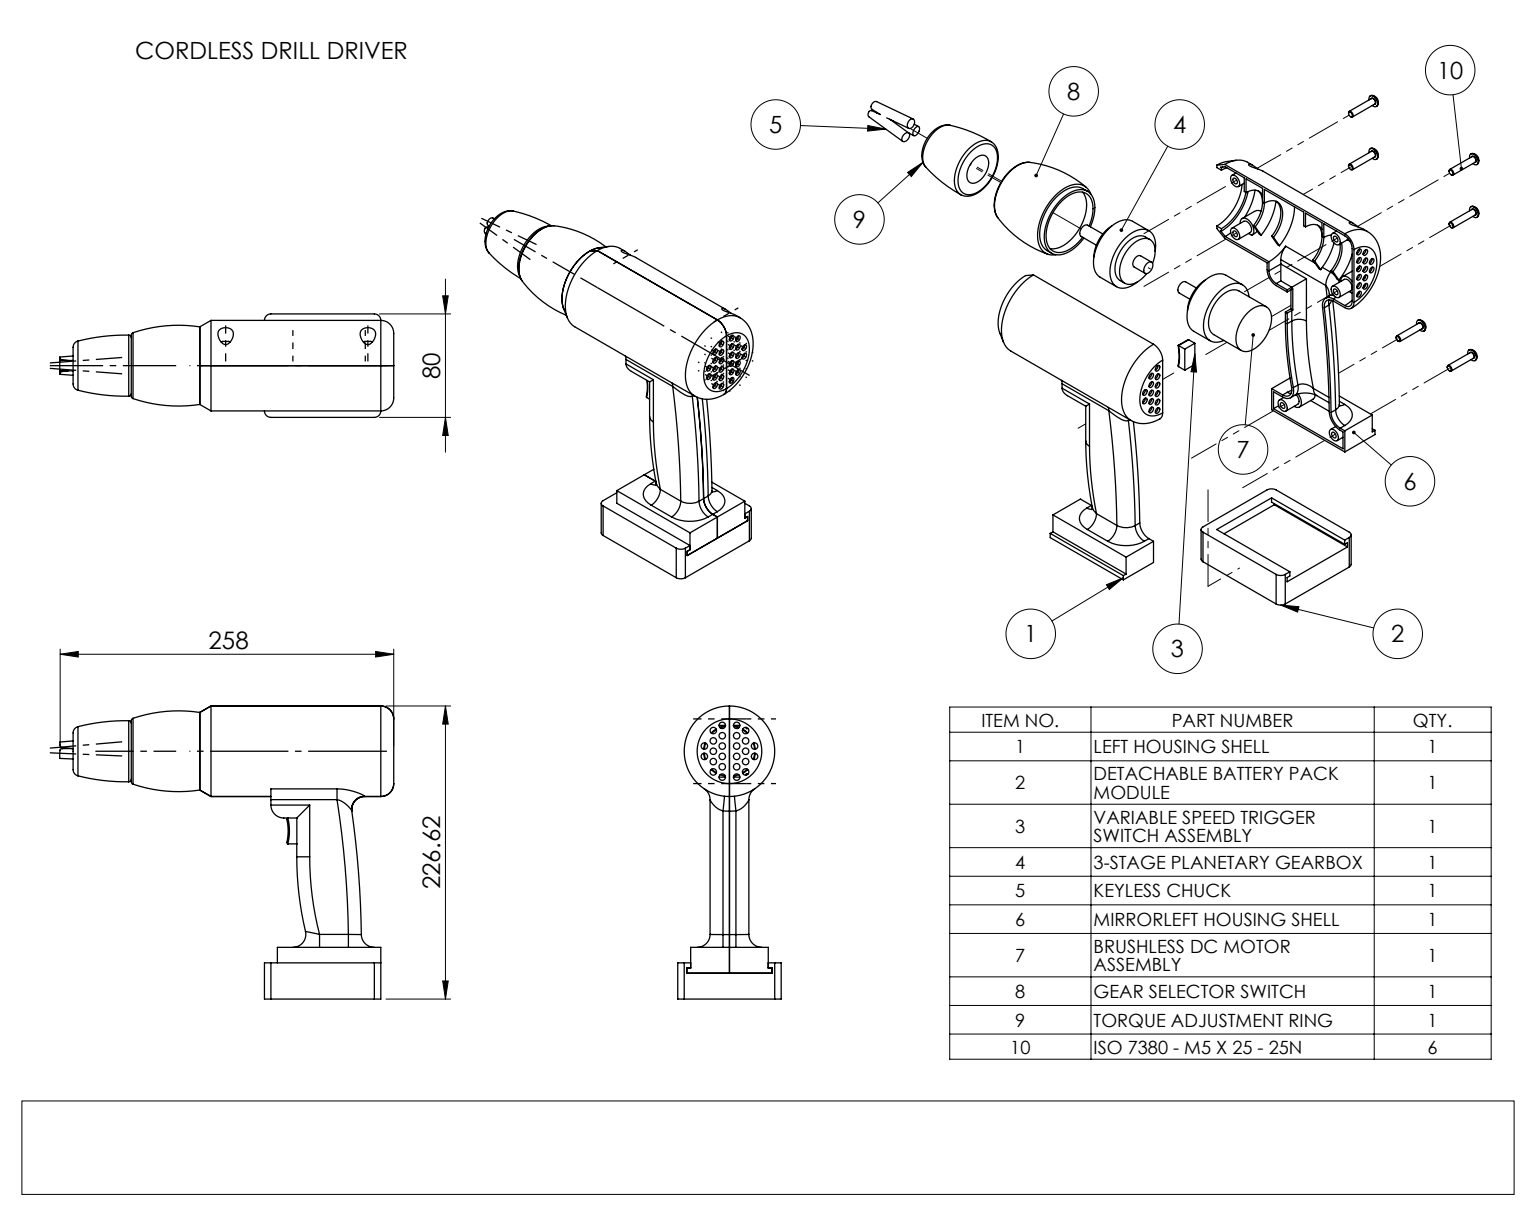
ISO-10303-21;
HEADER;
FILE_DESCRIPTION (('STEP AP214'),
    '1' );
FILE_NAME ('BR-801',
    '2026-10-05T20:22:16',
    ( '' ),
    ( '' ),
    'SwSTEP 2.0',
    'SolidWorks 2026',
    '' );
FILE_SCHEMA (( 'AUTOMOTIVE_DESIGN' ));
ENDSEC;

DATA;
#1 = B_SPLINE_CURVE_WITH_KNOTS ( 'NONE', 3,
 ( #12352, #9685, #8096, #1383, #14752, #16256, #12262, #13513, #2624, #1474, #13417, #8273, #9424, #10672, #226, #14828, #5538, #2709, #8188, #5630, #16442, #6792, #7929, #6603, #12185, #55, #13336, #5455, #10843, #10926, #4124, #11996, #2798, #16348, #13681, #6869, #9602, #15004, #9865, #16607, #8540, #3321, #16516, #15178, #7128, #4646, #4480, #11188, #15272, #15441 ),
 .UNSPECIFIED., .F., .F.,
 ( 4, 2, 2, 2, 2, 2, 2, 2, 2, 2, 2, 2, 2, 2, 2, 2, 2, 2, 2, 2, 2, 2, 2, 2, 4 ),
 ( 0.02172192739389853383, 0.02251948391625541862, 0.02331704043861230341, 0.02491215348332601748, 0.02650726652803973155, 0.02810237957275344908, 0.02969749261746715968, 0.03129260566218088069, 0.03209016218453770303, 0.03288771870689453231, 0.03328649696807296082, 0.03368527522925138240, 0.03448283175160819780, 0.03528038827396501320, 0.03567916653514340702, 0.03607794479632180085, 0.03687550131867862319, 0.03767305784103544553, 0.03847061436339226786, 0.03926817088574909020, 0.04086328393046270713, 0.04245839697517631711, 0.04405351001988992710, 0.04564862306460354402, 0.04724373610931716094 ),
 .UNSPECIFIED. ) ;
#2 = EDGE_CURVE ( 'NONE', #9188, #6176, #1844, .T. ) ;
#3 = AXIS2_PLACEMENT_3D ( 'NONE', #2045, #12839, #15664 ) ;
#4 = DIRECTION ( 'NONE',  ( 0.000000000000000000, 0.000000000000000000, -1.000000000000000000 ) ) ;
#5 = DIRECTION ( 'NONE',  ( 0.000000000000000000, 0.000000000000000000, 1.000000000000000000 ) ) ;
#6 = CARTESIAN_POINT ( 'NONE',  ( 27.15273249069231198, 18.00000000000000000, -20.88767039909325973 ) ) ;
#7 = CARTESIAN_POINT ( 'NONE',  ( 25.49876332522149625, 18.00000000000000000, -21.99427390110736624 ) ) ;
#8 = CYLINDRICAL_SURFACE ( 'NONE', #14336, 2.500000000000000444 ) ;
#9 = DIRECTION ( 'NONE',  ( -1.000000000000000000, 0.000000000000000000, 0.000000000000000000 ) ) ;
#10 = DIRECTION ( 'NONE',  ( -1.000000000000000000, -0.000000000000000000, -0.000000000000000000 ) ) ;
#11 = CARTESIAN_POINT ( 'NONE',  ( -70.00000000000000000, 171.6227766016838245, 0.000000000000000000 ) ) ;
#12 = ORIENTED_EDGE ( 'NONE', *, *, #6579, .T. ) ;
#13 = CARTESIAN_POINT ( 'NONE',  ( 16.03791926353974162, 127.7299327228906520, -9.742640703122631862 ) ) ;
#14 = CIRCLE ( 'NONE', #9896, 10.00000000000000178 ) ;
#15 = AXIS2_PLACEMENT_3D ( 'NONE', #2563, #7954, #5300 ) ;
#16 = ORIENTED_EDGE ( 'NONE', *, *, #13429, .F. ) ;
#17 = CARTESIAN_POINT ( 'NONE',  ( 196.0000000000000000, 191.6227766016837677, 3.071800142134975431 ) ) ;
#18 = CIRCLE ( 'NONE', #14435, 20.00000000000000355 ) ;
#19 = CYLINDRICAL_SURFACE ( 'NONE', #8941, 2.500000000000000444 ) ;
#20 = ORIENTED_EDGE ( 'NONE', *, *, #455, .F. ) ;
#21 = CARTESIAN_POINT ( 'NONE',  ( -12.77984573873758656, 20.00000000000230216, 11.87289823213939854 ) ) ;
#22 = CARTESIAN_POINT ( 'NONE',  ( 14.63750484765316706, 138.5418767416829837, 5.508738673615532377 ) ) ;
#23 = ORIENTED_EDGE ( 'NONE', *, *, #10609, .T. ) ;
#24 = CARTESIAN_POINT ( 'NONE',  ( 21.36708699129162881, 19.99999999999999645, 23.94811280430947420 ) ) ;
#25 = EDGE_CURVE ( 'NONE', #5251, #13584, #2714, .T. ) ;
#26 = AXIS2_PLACEMENT_3D ( 'NONE', #12707, #5981, #16782 ) ;
#27 = ORIENTED_EDGE ( 'NONE', *, *, #8063, .T. ) ;
#28 = AXIS2_PLACEMENT_3D ( 'NONE', #8615, #16596, #11271 ) ;
#29 = DIRECTION ( 'NONE',  ( 0.000000000000000000, 1.000000000000000000, 0.000000000000000000 ) ) ;
#30 = CARTESIAN_POINT ( 'NONE',  ( -15.00000000000002132, 100.0000000000000142, 4.999999999999999112 ) ) ;
#31 = DIRECTION ( 'NONE',  ( 0.000000000000000000, 0.000000000000000000, -1.000000000000000000 ) ) ;
#32 = CARTESIAN_POINT ( 'NONE',  ( -194.2319660531761656, 171.6227766016838245, -19.01029467089431080 ) ) ;
#33 = ADVANCED_FACE ( 'NONE', ( #8260 ), #11261, .F. ) ;
#34 = EDGE_CURVE ( 'NONE', #17370, #11003, #7190, .T. ) ;
#35 = ORIENTED_EDGE ( 'NONE', *, *, #2235, .F. ) ;
#36 = DIRECTION ( 'NONE',  ( -1.000000000000000000, 0.000000000000000000, 0.000000000000000000 ) ) ;
#37 = ORIENTED_EDGE ( 'NONE', *, *, #4762, .T. ) ;
#38 = CARTESIAN_POINT ( 'NONE',  ( -80.30638721710498373, 189.1234298779548624, -27.97726104294732963 ) ) ;
#39 = FACE_OUTER_BOUND ( 'NONE', #11505, .T. ) ;
#40 = AXIS2_PLACEMENT_3D ( 'NONE', #14825, #13678, #6691 ) ;
#41 = ORIENTED_EDGE ( 'NONE', *, *, #303, .F. ) ;
#42 = ORIENTED_EDGE ( 'NONE', *, *, #11841, .T. ) ;
#43 = ORIENTED_EDGE ( 'NONE', *, *, #9422, .T. ) ;
#44 = CARTESIAN_POINT ( 'NONE',  ( 9.986687348566183786, 132.8041431104223307, 14.33374896416919064 ) ) ;
#45 = ORIENTED_EDGE ( 'NONE', *, *, #7953, .F. ) ;
#46 = SHAPE_DEFINITION_REPRESENTATION ( #2904, #690 ) ;
#47 = CARTESIAN_POINT ( 'NONE',  ( -40.85786437626905609, 120.0000000000000142, 10.85786437626904721 ) ) ;
#48 = FACE_OUTER_BOUND ( 'NONE', #5615, .T. ) ;
#49 = PRODUCT_DEFINITION ( 'UNKNOWN', '', #15196, #232 ) ;
#50 = CARTESIAN_POINT ( 'NONE',  ( -48.00000000000000000, 143.0439382767972347, -16.49999999999984368 ) ) ;
#51 = AXIS2_PLACEMENT_3D ( 'NONE', #14892, #2772, #6847 ) ;
#52 = DIRECTION ( 'NONE',  ( 0.000000000000000000, 0.000000000000000000, -1.000000000000000000 ) ) ;
#53 = CARTESIAN_POINT ( 'NONE',  ( -80.79725519073433304, 151.5627461462769929, 26.20297826401936803 ) ) ;
#54 = ORIENTED_EDGE ( 'NONE', *, *, #3388, .T. ) ;
#55 = CARTESIAN_POINT ( 'NONE',  ( -79.71276265205243305, 202.6220268295897711, -16.24950730846250835 ) ) ;
#56 = CARTESIAN_POINT ( 'NONE',  ( 14.34366722128227067, 129.4994645064758174, 11.74322308516846647 ) ) ;
#57 = CARTESIAN_POINT ( 'NONE',  ( -95.00000000000000000, 171.6227766016838245, 0.000000000000000000 ) ) ;
#58 = CARTESIAN_POINT ( 'NONE',  ( -43.00000000000000000, 144.1839557653416080, 18.33333333333335702 ) ) ;
#59 = PLANE ( 'NONE',  #13735 ) ;
#60 = DIRECTION ( 'NONE',  ( 1.000000000000000000, 0.000000000000000000, 0.000000000000000000 ) ) ;
#61 = EDGE_CURVE ( 'NONE', #735, #11290, #4368, .T. ) ;
#62 = ORIENTED_EDGE ( 'NONE', *, *, #6340, .T. ) ;
#63 = FACE_OUTER_BOUND ( 'NONE', #17014, .T. ) ;
#64 = ORIENTED_EDGE ( 'NONE', *, *, #1601, .F. ) ;
#65 = SHAPE_REPRESENTATION_RELATIONSHIP ( 'NONE' , 'NONE' ,  #7924, #8036 ) ;
#66 = LINE ( 'NONE', #2892, #16980 ) ;
#67 = DIRECTION ( 'NONE',  ( 8.673617379884037937E-17, 0.000000000000000000, 1.000000000000000000 ) ) ;
#68 = DIRECTION ( 'NONE',  ( 0.000000000000000000, 0.000000000000000000, 1.000000000000000000 ) ) ;
#69 = CARTESIAN_POINT ( 'NONE',  ( 0.000000000000000000, 20.00000000000000000, 25.00000000000000000 ) ) ;
#70 = EDGE_LOOP ( 'NONE', ( #17465, #2421, #13202, #13512 ) ) ;
#71 = DIRECTION ( 'NONE',  ( -1.000000000000000000, 0.000000000000000000, 0.000000000000000000 ) ) ;
#72 = CARTESIAN_POINT ( 'NONE',  ( -48.00000000000000000, 191.6227766016837961, 1.224646799147353454E-15 ) ) ;
#73 = DIRECTION ( 'NONE',  ( 1.000000000000000000, 0.000000000000000000, 0.000000000000000000 ) ) ;
#74 =( NAMED_UNIT ( * ) PLANE_ANGLE_UNIT ( ) SI_UNIT ( $, .RADIAN. ) );
#75 = CARTESIAN_POINT ( 'NONE',  ( 15.93460003626540100, 136.8193095811535045, -3.708327557688629206 ) ) ;
#76 = ADVANCED_FACE ( 'NONE', ( #15069 ), #3033, .F. ) ;
#77 = EDGE_CURVE ( 'NONE', #13658, #4758, #14864, .T. ) ;
#78 = EDGE_CURVE ( 'NONE', #10896, #7127, #13853, .T. ) ;
#79 = ORIENTED_EDGE ( 'NONE', *, *, #12627, .T. ) ;
#80 = DIRECTION ( 'NONE',  ( 1.000000000000000000, 0.000000000000000000, 0.000000000000000000 ) ) ;
#81 = EDGE_CURVE ( 'NONE', #4275, #9730, #165, .T. ) ;
#82 = LINE ( 'NONE', #2908, #5241 ) ;
#83 = ORIENTED_EDGE ( 'NONE', *, *, #15385, .F. ) ;
#84 = CARTESIAN_POINT ( 'NONE',  ( -74.45226540305546337, 194.3303362407250177, -26.63481108765543581 ) ) ;
#85 = DIRECTION ( 'NONE',  ( -1.000000000000000000, -0.000000000000000000, -0.000000000000000000 ) ) ;
#86 = APPLICATION_CONTEXT ( 'automotive_design' ) ;
#87 = DIRECTION ( 'NONE',  ( 0.000000000000000000, 0.000000000000000000, 1.000000000000000000 ) ) ;
#88 = CARTESIAN_POINT ( 'NONE',  ( 24.94691999498327206, 18.00000000000000711, -22.32501294936691139 ) ) ;
#89 = CARTESIAN_POINT ( 'NONE',  ( 23.77503517897901375, 18.00000000000000000, -22.95135521423614833 ) ) ;
#90 = CARTESIAN_POINT ( 'NONE',  ( 37.50000000000000711, 196.6227766016838245, -35.00200000000000244 ) ) ;
#91 = LINE ( 'NONE', #4168, #1104 ) ;
#92 = CARTESIAN_POINT ( 'NONE',  ( 2.370000000000000551, 0.000000000000000000, 0.000000000000000000 ) ) ;
#93 = CARTESIAN_POINT ( 'NONE',  ( 26.85005685037350176, 141.4992599418080772, -17.82476597062854040 ) ) ;
#94 = ORIENTED_EDGE ( 'NONE', *, *, #1318, .F. ) ;
#95 = CARTESIAN_POINT ( 'NONE',  ( 6.927042533203191965, 134.0880917650273716, -15.00000000000000533 ) ) ;
#96 = EDGE_LOOP ( 'NONE', ( #1824, #2335, #11852, #6103 ) ) ;
#97 = DIRECTION ( 'NONE',  ( 0.000000000000000000, 0.000000000000000000, 1.000000000000000000 ) ) ;
#98 = CARTESIAN_POINT ( 'NONE',  ( 225.0000000000000000, 89.99999999999997158, -4.999999999999999112 ) ) ;
#99 = ORIENTED_EDGE ( 'NONE', *, *, #10624, .F. ) ;
#100 = PLANE ( 'NONE',  #16536 ) ;
#101 = LINE ( 'NONE', #8243, #15842 ) ;
#102 = VERTEX_POINT ( 'NONE', #8434 ) ;
#103 = DIRECTION ( 'NONE',  ( 0.000000000000000000, 0.000000000000000000, 1.000000000000000000 ) ) ;
#104 = ORIENTED_EDGE ( 'NONE', *, *, #3991, .F. ) ;
#105 = LINE ( 'NONE', #5601, #6122 ) ;
#106 = DIRECTION ( 'NONE',  ( -1.000000000000000000, 0.000000000000000000, 0.000000000000000000 ) ) ;
#107 = CARTESIAN_POINT ( 'NONE',  ( 33.99999999999998579, 9.999999999999998224, -35.00000000000000000 ) ) ;
#108 = ORIENTED_EDGE ( 'NONE', *, *, #12256, .F. ) ;
#109 = DIRECTION ( 'NONE',  ( -0.000000000000000000, -1.000000000000000000, -0.000000000000000000 ) ) ;
#110 = ORIENTED_EDGE ( 'NONE', *, *, #17517, .F. ) ;
#111 = LINE ( 'NONE', #8166, #1932 ) ;
#112 = EDGE_CURVE ( 'NONE', #17297, #3029, #16627, .T. ) ;
#113 = ORIENTED_EDGE ( 'NONE', *, *, #13886, .F. ) ;
#114 = EDGE_CURVE ( 'NONE', #730, #9326, #14586, .T. ) ;
#115 = CARTESIAN_POINT ( 'NONE',  ( -78.86500048027876630, 189.1866491494219815, -27.93804624201380804 ) ) ;
#116 = DIRECTION ( 'NONE',  ( 0.000000000000000000, 0.000000000000000000, 1.000000000000000000 ) ) ;
#117 =( BOUNDED_SURFACE ( )  B_SPLINE_SURFACE ( 3, 2, ( 
 ( #14255, #2119, #7358 ),
 ( #807, #6197, #12760 ),
 ( #632, #11415, #4699 ),
 ( #16827, #8771, #2299 ),
 ( #9106, #17259, #13450 ),
 ( #5135, #5041, #10344 ),
 ( #3799, #16120, #1322 ),
 ( #15926, #965, #13280 ),
 ( #13364, #6550, #2476 ),
 ( #14512, #14600, #10434 ),
 ( #15848, #1058, #6637 ),
 ( #11850, #2379, #3721 ),
 ( #6458, #16018, #11941 ),
 ( #8042, #15754, #7870 ),
 ( #7772, #5213, #10523 ),
 ( #10610, #6729, #9194 ),
 ( #13185, #1148, #17343 ),
 ( #3900, #9284, #12126 ),
 ( #3631, #4951, #3997 ),
 ( #14695, #11759, #2575 ),
 ( #7961, #1231, #9021 ),
 ( #14436, #7692, #9377 ),
 ( #13099, #12030, #17435 ),
 ( #6362, #5310, #17170 ),
 ( #14779, #10704, #2651 ),
 ( #13711, #13812, #9715 ),
 ( #11051, #256, #7075 ),
 ( #1415, #4329, #341 ),
 ( #4156, #8392, #9541 ),
 ( #8220, #1582, #3039 ) ),
 .UNSPECIFIED., .F., .F., .F. ) 
 B_SPLINE_SURFACE_WITH_KNOTS ( ( 4, 2, 2, 2, 2, 2, 2, 2, 2, 2, 2, 2, 2, 2, 4 ),
 ( 3, 3 ),
 ( 0.01165250788892075590, 0.01579789672993321681, 0.01787059115043944726, 0.01890693836069256423, 0.01994328557094567772, 0.02408867441195813863, 0.02616136883246436562, 0.02823406325297059608, 0.03030675767347682653, 0.03237945209398305352, 0.03652484093499551443, 0.03859753535550174142, 0.03963388256575485491, 0.04067022977600797534, 0.04481561861702043625 ),
 ( 0.000000000000000000, 1.000000000000000000 ),
 .UNSPECIFIED. ) 
 GEOMETRIC_REPRESENTATION_ITEM ( )  RATIONAL_B_SPLINE_SURFACE ( (
 ( 1.000000000000000000, 0.8819171036881968684, 1.000000000000000000),
 ( 1.000000000000000000, 0.8793942645247271317, 1.000000000000000000),
 ( 1.000000000000000000, 0.8749458316895473153, 1.000000000000000000),
 ( 1.000000000000000000, 0.8656814021268807169, 1.000000000000000000),
 ( 1.000000000000000000, 0.8621600075895787807, 1.000000000000000000),
 ( 1.000000000000000000, 0.8562492930711512740, 1.000000000000000000),
 ( 1.000000000000000000, 0.8541736901086096623, 1.000000000000000000),
 ( 1.000000000000000000, 0.8498659178638878764, 1.000000000000000000),
 ( 1.000000000000000000, 0.8476283308600994770, 1.000000000000000000),
 ( 1.000000000000000000, 0.8360458749413697266, 1.000000000000000000),
 ( 1.000000000000000000, 0.8255221978283152628, 1.000000000000000000),
 ( 1.000000000000000000, 0.8082270345000643896, 1.000000000000000000),
 ( 1.000000000000000000, 0.8022128341713220534, 1.000000000000000000),
 ( 1.000000000000000000, 0.7899684886175323273, 1.000000000000000000),
 ( 1.000000000000000000, 0.7837128169312477244, 1.000000000000000000),
 ( 1.000000000000000000, 0.7710263478628327505, 1.000000000000000000),
 ( 1.000000000000000000, 0.7645952338537677084, 1.000000000000000000),
 ( 1.000000000000000000, 0.7516613202047349729, 1.000000000000000000),
 ( 1.000000000000000000, 0.7451386183435962929, 1.000000000000000000),
 ( 1.000000000000000000, 0.7257808243687768890, 1.000000000000000000),
 ( 1.000000000000000000, 0.7133953845776382918, 1.000000000000000000),
 ( 1.000000000000000000, 0.6965170042221158209, 1.000000000000000000),
 ( 1.000000000000000000, 0.6911767420096451842, 1.000000000000000000),
 ( 1.000000000000000000, 0.6837405640632109316, 1.000000000000000000),
 ( 1.000000000000000000, 0.6813577907324296357, 1.000000000000000000),
 ( 1.000000000000000000, 0.6768117804540668692, 1.000000000000000000),
 ( 1.000000000000000000, 0.6746439590912666207, 1.000000000000000000),
 ( 1.000000000000000000, 0.6645663254999827352, 1.000000000000000000),
 ( 1.000000000000000000, 0.6588263891900785207, 1.000000000000000000),
 ( 1.000000000000000000, 0.6558243695371216431, 1.000000000000000000) ) ) 
 REPRESENTATION_ITEM ( '' )  SURFACE ( )  );
#118 = VERTEX_POINT ( 'NONE', #16766 ) ;
#119 = ORIENTED_EDGE ( 'NONE', *, *, #7483, .T. ) ;
#120 = ORIENTED_EDGE ( 'NONE', *, *, #14822, .T. ) ;
#121 = AXIS2_PLACEMENT_3D ( 'NONE', #12390, #5748, #16650 ) ;
#122 = AXIS2_PLACEMENT_3D ( 'NONE', #11876, #6482, #6572 ) ;
#123 = PLANE ( 'NONE',  #15795 ) ;
#124 = CARTESIAN_POINT ( 'NONE',  ( 10.15450428991780285, 132.7081580017661224, 14.27405243007192581 ) ) ;
#125 = ADVANCED_FACE ( 'NONE', ( #16843, #6296, #6218, #3209, #822 ), #15422, .T. ) ;
#126 = ORIENTED_EDGE ( 'NONE', *, *, #14248, .F. ) ;
#127 = CARTESIAN_POINT ( 'NONE',  ( 27.99999999999998224, 9.999999999999998224, -18.74999999999999645 ) ) ;
#128 = DIRECTION ( 'NONE',  ( -1.000000000000000000, -0.000000000000000000, -0.000000000000000000 ) ) ;
#129 = DIRECTION ( 'NONE',  ( 0.000000000000000000, 0.000000000000000000, 1.000000000000000000 ) ) ;
#130 = CARTESIAN_POINT ( 'NONE',  ( 22.12508471281541134, 29.85770821936580433, -8.546410110412809402 ) ) ;
#131 = CARTESIAN_POINT ( 'NONE',  ( 39.99999999999998579, 5.659323622547703371E-16, -33.00000000000000000 ) ) ;
#132 = CARTESIAN_POINT ( 'NONE',  ( -24.99999999999999289, 100.0000000000000142, 0.000000000000000000 ) ) ;
#133 = CIRCLE ( 'NONE', #1548, 2.499999999999998668 ) ;
#134 = VERTEX_POINT ( 'NONE', #6129 ) ;
#135 = CYLINDRICAL_SURFACE ( 'NONE', #5598, 8.000000000000007105 ) ;
#136 = CIRCLE ( 'NONE', #10306, 12.00000000000000000 ) ;
#137 = CARTESIAN_POINT ( 'NONE',  ( 34.80468147095351128, 20.00000000000000000, -7.619145204522578041 ) ) ;
#138 = ADVANCED_FACE ( 'NONE', ( #7376, #14017 ), #15677, .T. ) ;
#139 = LINE ( 'NONE', #14923, #9291 ) ;
#140 = FACE_OUTER_BOUND ( 'NONE', #14292, .T. ) ;
#141 = ORIENTED_EDGE ( 'NONE', *, *, #16389, .F. ) ;
#142 = CARTESIAN_POINT ( 'NONE',  ( -82.50000000000001421, 196.6227766016838245, 0.000000000000000000 ) ) ;
#143 = ORIENTED_EDGE ( 'NONE', *, *, #14951, .F. ) ;
#144 = EDGE_CURVE ( 'NONE', #16894, #7251, #3853, .T. ) ;
#145 = DIRECTION ( 'NONE',  ( 0.000000000000000000, -0.000000000000000000, -1.000000000000000000 ) ) ;
#146 = EDGE_CURVE ( 'NONE', #17383, #9593, #6108, .T. ) ;
#147 = ORIENTED_EDGE ( 'NONE', *, *, #10920, .T. ) ;
#148 =( LENGTH_UNIT ( ) NAMED_UNIT ( * ) SI_UNIT ( .MILLI., .METRE. ) );
#149 = CARTESIAN_POINT ( 'NONE',  ( 15.95607457768013404, 136.6882381644216196, -2.475222843548684715 ) ) ;
#150 = LINE ( 'NONE', #5809, #16568 ) ;
#151 = CARTESIAN_POINT ( 'NONE',  ( 1.559999999999998943, 1.732050807568885631, 0.000000000000000000 ) ) ;
#152 = VERTEX_POINT ( 'NONE', #7624 ) ;
#153 = CYLINDRICAL_SURFACE ( 'NONE', #9538, 24.99999999999999645 ) ;
#154 = CARTESIAN_POINT ( 'NONE',  ( 196.0000000000000000, 175.6227766016838530, 21.92820660268601074 ) ) ;
#155 = EDGE_CURVE ( 'NONE', #4227, #5635, #15763, .T. ) ;
#156 = CARTESIAN_POINT ( 'NONE',  ( -3.000000000000000888, 171.6227766016838245, 0.000000000000000000 ) ) ;
#157 = STYLED_ITEM ( 'NONE', ( #14231 ), #11475 ) ;
#158 = CIRCLE ( 'NONE', #16310, 33.00000000000000000 ) ;
#159 = CARTESIAN_POINT ( 'NONE',  ( 20.41303537792882139, 140.1262507166239573, -15.26811025958205015 ) ) ;
#160 = VERTEX_POINT ( 'NONE', #11356 ) ;
#161 = DIRECTION ( 'NONE',  ( 0.000000000000000000, 0.000000000000000000, -1.000000000000000000 ) ) ;
#162 = FACE_OUTER_BOUND ( 'NONE', #7033, .T. ) ;
#163 = EDGE_LOOP ( 'NONE', ( #2201, #7278 ) ) ;
#164 = CARTESIAN_POINT ( 'NONE',  ( -76.63222342921277175, 191.6397216241467163, -28.71272404723380234 ) ) ;
#165 = CIRCLE ( 'NONE', #16002, 2.500000000000002220 ) ;
#166 = AXIS2_PLACEMENT_3D ( 'NONE', #4042, #9504, #12180 ) ;
#167 = CARTESIAN_POINT ( 'NONE',  ( -7.379000772444994638, 30.00000000000000000, 25.00000000000000000 ) ) ;
#168 = CIRCLE ( 'NONE', #8369, 12.00000000000000000 ) ;
#169 = DIRECTION ( 'NONE',  ( -1.000000000000000000, -0.000000000000000000, 0.000000000000000000 ) ) ;
#170 = CARTESIAN_POINT ( 'NONE',  ( 17.00000000000000000, 154.3022685259950038, 9.999999999999900524 ) ) ;
#171 = CARTESIAN_POINT ( 'NONE',  ( -40.00000000000000000, 8.000000000000000000, -40.00000000000000000 ) ) ;
#172 = CARTESIAN_POINT ( 'NONE',  ( 15.46067906867578046, 29.98929614515185804, 13.00000000000000533 ) ) ;
#173 = ADVANCED_FACE ( 'NONE', ( #16682 ), #11434, .F. ) ;
#174 = EDGE_CURVE ( 'NONE', #6874, #11959, #3395, .T. ) ;
#175 = FACE_OUTER_BOUND ( 'NONE', #10777, .T. ) ;
#176 = EDGE_CURVE ( 'NONE', #5792, #4284, #10914, .T. ) ;
#177 = DIRECTION ( 'NONE',  ( 0.000000000000000000, -1.000000000000000000, 0.000000000000000000 ) ) ;
#178 = ORIENTED_EDGE ( 'NONE', *, *, #2632, .F. ) ;
#179 = CARTESIAN_POINT ( 'NONE',  ( 49.99999999999998579, 187.6227766016837961, 12.50000337241049309 ) ) ;
#180 = EDGE_LOOP ( 'NONE', ( #8241, #14719, #12649, #3237 ) ) ;
#181 = CARTESIAN_POINT ( 'NONE',  ( -50.00000000000000000, 171.6227766016838245, 0.000000000000000000 ) ) ;
#182 = CIRCLE ( 'NONE', #5556, 239.9999999999999716 ) ;
#183 = AXIS2_PLACEMENT_3D ( 'NONE', #7714, #6580, #13125 ) ;
#184 = CARTESIAN_POINT ( 'NONE',  ( -50.00000000000000000, 204.6227766016838245, 2.020667218593133100E-15 ) ) ;
#185 = VECTOR ( 'NONE', #14301, 1000.000000000000114 ) ;
#186 = ORIENTED_EDGE ( 'NONE', *, *, #12034, .F. ) ;
#187 = CARTESIAN_POINT ( 'NONE',  ( -25.16839285024614625, 19.99999999999999645, 15.12082343620048519 ) ) ;
#188 = AXIS2_PLACEMENT_3D ( 'NONE', #16749, #13998, #10087 ) ;
#189 = DIRECTION ( 'NONE',  ( 0.000000000000000000, 1.000000000000000000, 0.000000000000000000 ) ) ;
#190 = VERTEX_POINT ( 'NONE', #15337 ) ;
#191 = CARTESIAN_POINT ( 'NONE',  ( 36.34904889156061358, 150.6223998522366685, -25.45681811525070515 ) ) ;
#192 = ORIENTED_EDGE ( 'NONE', *, *, #2912, .T. ) ;
#193 = CARTESIAN_POINT ( 'NONE',  ( -95.00000000000000000, 171.6227766016838245, 0.000000000000000000 ) ) ;
#194 = CARTESIAN_POINT ( 'NONE',  ( -40.00000000000000000, 4.000000000000000000, -30.00000000000000711 ) ) ;
#195 = DIRECTION ( 'NONE',  ( 0.1091791256177803149, 0.9940220915700701543, 0.000000000000000000 ) ) ;
#196 = EDGE_LOOP ( 'NONE', ( #16642, #10984, #15395, #3760 ) ) ;
#197 = EDGE_CURVE ( 'NONE', #6224, #17297, #182, .T. ) ;
#198 = VECTOR ( 'NONE', #10876, 1000.000000000000000 ) ;
#199 = CYLINDRICAL_SURFACE ( 'NONE', #1827, 5.000000000000000888 ) ;
#200 = AXIS2_PLACEMENT_3D ( 'NONE', #10939, #4055, #145 ) ;
#201 = ORIENTED_EDGE ( 'NONE', *, *, #8299, .T. ) ;
#202 = FACE_OUTER_BOUND ( 'NONE', #3833, .T. ) ;
#203 = ORIENTED_EDGE ( 'NONE', *, *, #13054, .T. ) ;
#204 = CARTESIAN_POINT ( 'NONE',  ( -87.34717144291671787, 195.0632477915243896, -23.23525722188765741 ) ) ;
#205 = LINE ( 'NONE', #13586, #10347 ) ;
#206 = B_SPLINE_CURVE_WITH_KNOTS ( 'NONE', 3,
 ( #3287, #16669, #445, #365, #283, #11345, #15732, #8689, #8323, #15407, #4447, #11249, #548, #7099, #5687, #9833, #14096, #7178, #17064, #1960, #11419, #12580, #4538, #1702, #8592, #1874 ),
 .UNSPECIFIED., .F., .F.,
 ( 4, 2, 2, 2, 2, 2, 2, 2, 2, 2, 2, 2, 4 ),
 ( 0.000000000000000000, 0.002002783134349999609, 0.004005566268699999218, 0.008011132537399998435, 0.01001391567174999414, 0.01201669880609998985, 0.01602226507479997952, 0.01802504820914997002, 0.02002783134349995706, 0.02403339761219993806, 0.02603618074654992856, 0.02803896388089991906, 0.03204453014959990353 ),
 .UNSPECIFIED. ) ;
#207 = CARTESIAN_POINT ( 'NONE',  ( 48.00000000000000711, 175.6227766016838245, -5.571800142134975431 ) ) ;
#208 = ORIENTED_EDGE ( 'NONE', *, *, #12480, .F. ) ;
#209 = VERTEX_POINT ( 'NONE', #8951 ) ;
#210 = CARTESIAN_POINT ( 'NONE',  ( 15.00000000000000000, 204.6227766016838245, -2.020667218593133100E-15 ) ) ;
#211 = AXIS2_PLACEMENT_3D ( 'NONE', #6627, #17422, #13266 ) ;
#212 = CARTESIAN_POINT ( 'NONE',  ( 17.58250999372313927, 125.2198453307267414, 1.671679122699602171 ) ) ;
#213 = DIRECTION ( 'NONE',  ( -1.000000000000000000, 0.000000000000000000, 0.000000000000000000 ) ) ;
#214 = DIRECTION ( 'NONE',  ( 0.000000000000000000, -1.000000000000000000, -6.123233995736762338E-17 ) ) ;
#215 = CIRCLE ( 'NONE', #1923, 5.000000000000018652 ) ;
#216 = VERTEX_POINT ( 'NONE', #8789 ) ;
#217 = SHAPE_DEFINITION_REPRESENTATION ( #9683, #10772 ) ;
#218 = DIRECTION ( 'NONE',  ( 1.000000000000000000, 0.000000000000000000, -0.000000000000000000 ) ) ;
#219 = ADVANCED_FACE ( 'NONE', ( #14195 ), #2057, .T. ) ;
#220 = CARTESIAN_POINT ( 'NONE',  ( 32.50000000000000711, 146.6227766016838245, -16.00000000000000000 ) ) ;
#221 = CARTESIAN_POINT ( 'NONE',  ( 17.51497691750854813, 29.94811823131043127, -12.57651788136221072 ) ) ;
#222 = CARTESIAN_POINT ( 'NONE',  ( -40.00000000000000000, 0.000000000000000000, -33.00000000000000711 ) ) ;
#223 = CARTESIAN_POINT ( 'NONE',  ( 27.44407568426044364, 136.8394969516870958, 3.888888888888887063 ) ) ;
#224 = PRODUCT_DEFINITION_SHAPE ( 'NONE', 'NONE',  #17527 ) ;
#225 = ORIENTED_EDGE ( 'NONE', *, *, #16801, .F. ) ;
#226 = CARTESIAN_POINT ( 'NONE',  ( -83.14616744761717371, 201.7487681645689577, -17.82060658420953203 ) ) ;
#227 = DIRECTION ( 'NONE',  ( 0.000000000000000000, 0.000000000000000000, 1.000000000000000000 ) ) ;
#228 = CARTESIAN_POINT ( 'NONE',  ( -72.50000000000002842, 146.6227766016838245, -35.00200000000000244 ) ) ;
#229 = CARTESIAN_POINT ( 'NONE',  ( -208.1430079281944074, 172.4097984991905150, 5.932774073184737595 ) ) ;
#230 = VECTOR ( 'NONE', #15433, 1000.000000000000000 ) ;
#231 = CARTESIAN_POINT ( 'NONE',  ( -45.00000000000000000, 122.0000000000000142, 15.00000000000000000 ) ) ;
#232 = PRODUCT_DEFINITION_CONTEXT ( 'detailed design', #10711, 'design' ) ;
#233 = VERTEX_POINT ( 'NONE', #10201 ) ;
#234 = CARTESIAN_POINT ( 'NONE',  ( 48.00000000000000000, 171.6227766016838245, 0.000000000000000000 ) ) ;
#235 = EDGE_LOOP ( 'NONE', ( #13574, #321, #10866, #12718 ) ) ;
#236 = LINE ( 'NONE', #5641, #6716 ) ;
#237 = EDGE_LOOP ( 'NONE', ( #1431, #15859, #12881, #16657, #10889, #7991, #12906, #8862 ) ) ;
#238 = AXIS2_PLACEMENT_3D ( 'NONE', #16301, #6473, #17358 ) ;
#239 = CARTESIAN_POINT ( 'NONE',  ( 196.0000000000000000, 179.6227766016838245, 15.00000337241049486 ) ) ;
#240 = EDGE_CURVE ( 'NONE', #15883, #846, #6193, .T. ) ;
#241 = AXIS2_PLACEMENT_3D ( 'NONE', #3615, #7420, #699 ) ;
#242 = CARTESIAN_POINT ( 'NONE',  ( -95.00000000000000000, 171.6227766016838245, 0.000000000000000000 ) ) ;
#243 = VERTEX_POINT ( 'NONE', #13302 ) ;
#244 = CARTESIAN_POINT ( 'NONE',  ( -100.0000000000000000, 143.9321776784423150, -5.086680500673126297E-15 ) ) ;
#245 = ADVANCED_FACE ( 'NONE', ( #10458, #10362 ), #15773, .T. ) ;
#246 = DIRECTION ( 'NONE',  ( -0.000000000000000000, -0.000000000000000000, -1.000000000000000000 ) ) ;
#247 = FACE_BOUND ( 'NONE', #9621, .T. ) ;
#248 = ADVANCED_FACE ( 'NONE', ( #14797, #17095 ), #7707, .F. ) ;
#249 = FILL_AREA_STYLE_COLOUR ( '', #15123 ) ;
#250 = EDGE_CURVE ( 'NONE', #2500, #6282, #1348, .T. ) ;
#251 = AXIS2_PLACEMENT_3D ( 'NONE', #3268, #2197, #881 ) ;
#252 = CIRCLE ( 'NONE', #11000, 2.500000000000000000 ) ;
#253 = CARTESIAN_POINT ( 'NONE',  ( 14.17453072134883030, 137.9246278893784847, -11.09209212451273352 ) ) ;
#254 = VERTEX_POINT ( 'NONE', #2317 ) ;
#255 = FACE_BOUND ( 'NONE', #9759, .T. ) ;
#256 = CARTESIAN_POINT ( 'NONE',  ( 14.12141184870282196, 138.6801925718470443, -3.743222489502411321 ) ) ;
#257 = ORIENTED_EDGE ( 'NONE', *, *, #3098, .T. ) ;
#258 = DIRECTION ( 'NONE',  ( 0.000000000000000000, 0.000000000000000000, 1.000000000000000000 ) ) ;
#259 = CARTESIAN_POINT ( 'NONE',  ( -80.44925623706835438, 190.6352453962669813, -29.38582951075080985 ) ) ;
#260 = DIRECTION ( 'NONE',  ( -0.000000000000000000, -0.000000000000000000, -1.000000000000000000 ) ) ;
#261 = CIRCLE ( 'NONE', #1953, 5.000000000000007994 ) ;
#262 = CIRCLE ( 'NONE', #2818, 2.499999999999998668 ) ;
#263 = CARTESIAN_POINT ( 'NONE',  ( -43.00000000000000000, 130.0000000000000000, -15.00000000000000000 ) ) ;
#264 = AXIS2_PLACEMENT_3D ( 'NONE', #14224, #8819, #502 ) ;
#265 = DIRECTION ( 'NONE',  ( -0.000000000000000000, -0.000000000000000000, -1.000000000000000000 ) ) ;
#266 = CARTESIAN_POINT ( 'NONE',  ( 19.82112781281243130, 29.90253658286262350, 11.35562597552217845 ) ) ;
#267 = CARTESIAN_POINT ( 'NONE',  ( 11.38015211399644500, 143.8700659084811093, -17.85516819212570638 ) ) ;
#268 = CARTESIAN_POINT ( 'NONE',  ( 34.99999999999999289, -20.00000000000000000, 39.99999999999998579 ) ) ;
#269 = ORIENTED_EDGE ( 'NONE', *, *, #1597, .F. ) ;
#270 = ORIENTED_EDGE ( 'NONE', *, *, #12627, .F. ) ;
#271 = CARTESIAN_POINT ( 'NONE',  ( 24.41196201396447663, 19.99999999999999645, -8.570466955472159754 ) ) ;
#272 = CIRCLE ( 'NONE', #13562, 28.26633746182136164 ) ;
#273 = VECTOR ( 'NONE', #8822, 1000.000000000000000 ) ;
#274 = CARTESIAN_POINT ( 'NONE',  ( 24.00000000000000000, 196.6227766016838245, -16.00000000000000000 ) ) ;
#275 = ORIENTED_EDGE ( 'NONE', *, *, #16105, .F. ) ;
#276 = CARTESIAN_POINT ( 'NONE',  ( -15.53366225407947354, 31.76144936975385136, 11.66511309525283835 ) ) ;
#277 = CIRCLE ( 'NONE', #6204, 20.00000000000000355 ) ;
#278 = DIRECTION ( 'NONE',  ( 1.000000000000000000, 0.000000000000000000, 0.000000000000000000 ) ) ;
#279 = EDGE_CURVE ( 'NONE', #3972, #817, #6479, .T. ) ;
#280 = ORIENTED_EDGE ( 'NONE', *, *, #8979, .F. ) ;
#281 = EDGE_CURVE ( 'NONE', #6275, #15920, #15863, .T. ) ;
#282 = CARTESIAN_POINT ( 'NONE',  ( -50.00000000000000000, 171.6227766016838245, 0.000000000000000000 ) ) ;
#283 = CARTESIAN_POINT ( 'NONE',  ( -27.70723240392776887, 18.00000000000000000, 8.328409877367404235 ) ) ;
#284 = CARTESIAN_POINT ( 'NONE',  ( -68.00000000000000000, 171.6227766016838245, 24.99999999999999289 ) ) ;
#285 = DIRECTION ( 'NONE',  ( 0.000000000000000000, 0.000000000000000000, -1.000000000000000000 ) ) ;
#286 = AXIS2_PLACEMENT_3D ( 'NONE', #5190, #14314, #1029 ) ;
#287 = CIRCLE ( 'NONE', #5084, 23.57392898041429774 ) ;
#288 = LINE ( 'NONE', #8596, #3725 ) ;
#289 = PLANE ( 'NONE',  #9740 ) ;
#290 = CIRCLE ( 'NONE', #10181, 33.00000000000000000 ) ;
#291 = DIRECTION ( 'NONE',  ( -1.000000000000000000, 0.000000000000000000, 0.000000000000000000 ) ) ;
#292 = EDGE_LOOP ( 'NONE', ( #6190, #15449, #12115, #5130, #6244, #17037, #12475 ) ) ;
#293 = CARTESIAN_POINT ( 'NONE',  ( 225.0000000000000000, 89.99999999999997158, -4.999999999999999112 ) ) ;
#294 = EDGE_LOOP ( 'NONE', ( #280, #3412, #14427, #14815 ) ) ;
#295 = CARTESIAN_POINT ( 'NONE',  ( -72.55951795904178425, 195.6584727333609521, -22.61345334826514630 ) ) ;
#296 = FACE_BOUND ( 'NONE', #6496, .T. ) ;
#297 = DIRECTION ( 'NONE',  ( 0.000000000000000000, 0.000000000000000000, 1.000000000000000000 ) ) ;
#298 = ORIENTED_EDGE ( 'NONE', *, *, #12256, .T. ) ;
#299 = EDGE_LOOP ( 'NONE', ( #9917, #12342, #13408, #14524 ) ) ;
#300 = CARTESIAN_POINT ( 'NONE',  ( -90.80384757729339640, 204.6227766016838245, 0.000000000000000000 ) ) ;
#301 = CIRCLE ( 'NONE', #9619, 24.99999999999999645 ) ;
#302 = EDGE_CURVE ( 'NONE', #14819, #8809, #14878, .T. ) ;
#303 = EDGE_CURVE ( 'NONE', #12797, #10037, #6701, .T. ) ;
#304 = FACE_OUTER_BOUND ( 'NONE', #8211, .T. ) ;
#305 = EDGE_CURVE ( 'NONE', #13136, #4801, #3737, .T. ) ;
#306 = CARTESIAN_POINT ( 'NONE',  ( 16.12877328687227774, 136.8349817083154676, 4.209125965272636272 ) ) ;
#307 = ORIENTED_EDGE ( 'NONE', *, *, #3862, .T. ) ;
#308 = PLANE ( 'NONE',  #8782 ) ;
#309 = DIRECTION ( 'NONE',  ( -0.000000000000000000, -0.000000000000000000, -1.000000000000000000 ) ) ;
#310 = CARTESIAN_POINT ( 'NONE',  ( -50.00000000000000000, 171.6227766016838245, 0.000000000000000000 ) ) ;
#311 = CARTESIAN_POINT ( 'NONE',  ( -32.66708739526796279, 119.0000000000141824, -4.722170599054655860 ) ) ;
#312 = FACE_OUTER_BOUND ( 'NONE', #3125, .T. ) ;
#313 = VERTEX_POINT ( 'NONE', #2399 ) ;
#314 = CARTESIAN_POINT ( 'NONE',  ( -31.89848094669885725, 100.0271397714182342, 5.500000000000000000 ) ) ;
#315 = CIRCLE ( 'NONE', #13889, 10.00000000000000178 ) ;
#316 = FACE_OUTER_BOUND ( 'NONE', #16097, .T. ) ;
#317 = DIRECTION ( 'NONE',  ( -1.000000000000000000, 0.000000000000000000, 0.000000000000000000 ) ) ;
#318 = CARTESIAN_POINT ( 'NONE',  ( -45.00000000000000000, 130.0000000000000000, 0.000000000000000000 ) ) ;
#319 = ORIENTED_EDGE ( 'NONE', *, *, #15425, .T. ) ;
#320 = EDGE_CURVE ( 'NONE', #5614, #12465, #7243, .T. ) ;
#321 = ORIENTED_EDGE ( 'NONE', *, *, #1465, .F. ) ;
#322 = PLANE ( 'NONE',  #5083 ) ;
#323 = ORIENTED_EDGE ( 'NONE', *, *, #15869, .T. ) ;
#324 = DIRECTION ( 'NONE',  ( 0.8571673013836870192, 1.049727191973306873E-16, -0.5150380737757234151 ) ) ;
#325 = AXIS2_PLACEMENT_3D ( 'NONE', #12063, #5342, #16056 ) ;
#326 = ORIENTED_EDGE ( 'NONE', *, *, #14886, .T. ) ;
#327 = PRESENTATION_STYLE_ASSIGNMENT (( #16528 ) ) ;
#328 = CARTESIAN_POINT ( 'NONE',  ( -16.30611068361787019, 32.76923076923078781, -4.999999999999999112 ) ) ;
#329 = LINE ( 'NONE', #4059, #732 ) ;
#330 = DIRECTION ( 'NONE',  ( 0.000000000000000000, 0.000000000000000000, 1.000000000000000000 ) ) ;
#331 = CARTESIAN_POINT ( 'NONE',  ( -31.66708739526795924, 120.0000000000000284, -5.500000000000000000 ) ) ;
#332 = EDGE_LOOP ( 'NONE', ( #9563, #15113 ) ) ;
#333 = CARTESIAN_POINT ( 'NONE',  ( -100.0000000000000000, 171.6227766016838245, 0.000000000000000000 ) ) ;
#334 = LINE ( 'NONE', #11212, #17228 ) ;
#335 = FACE_BOUND ( 'NONE', #8357, .T. ) ;
#336 = ADVANCED_FACE ( 'NONE', ( #9394 ), #7794, .F. ) ;
#337 = EDGE_CURVE ( 'NONE', #3754, #14218, #4437, .T. ) ;
#338 = CARTESIAN_POINT ( 'NONE',  ( 25.02538947967125793, 138.3580044269788800, -10.92703196337285299 ) ) ;
#339 = ORIENTED_EDGE ( 'NONE', *, *, #6159, .F. ) ;
#340 = CARTESIAN_POINT ( 'NONE',  ( -74.59180618087658843, 149.2475623141791061, -26.91697313366100985 ) ) ;
#341 = CARTESIAN_POINT ( 'NONE',  ( 27.25143353317894324, 139.0964629073462220, -5.659441210211040740 ) ) ;
#342 = ORIENTED_EDGE ( 'NONE', *, *, #14528, .T. ) ;
#343 = FILL_AREA_STYLE_COLOUR ( '', #7574 ) ;
#344 = CARTESIAN_POINT ( 'NONE',  ( -77.78509460342800708, 191.0296277843087296, -29.12775510238319399 ) ) ;
#345 = EDGE_CURVE ( 'NONE', #10903, #313, #5234, .T. ) ;
#346 = DIRECTION ( 'NONE',  ( 0.000000000000000000, 0.000000000000000000, -1.000000000000000000 ) ) ;
#347 = CARTESIAN_POINT ( 'NONE',  ( 25.75727093772393061, 193.9598103731634637, 24.29383909379279061 ) ) ;
#348 = CARTESIAN_POINT ( 'NONE',  ( -116.4755503550297107, 171.6227766016838245, 0.000000000000000000 ) ) ;
#349 = CARTESIAN_POINT ( 'NONE',  ( 0.000000000000000000, 3.061616997868382155E-16, -2.499999999999999112 ) ) ;
#350 = CARTESIAN_POINT ( 'NONE',  ( -50.00000000000000000, 171.6227766016838245, 24.99999999999999289 ) ) ;
#351 = CARTESIAN_POINT ( 'NONE',  ( -79.90458729923355463, 201.6232707959690060, 13.74664867617476460 ) ) ;
#352 = DIRECTION ( 'NONE',  ( 1.000000000000000000, 0.000000000000000000, 0.000000000000000000 ) ) ;
#353 = ORIENTED_EDGE ( 'NONE', *, *, #661, .F. ) ;
#354 = ORIENTED_EDGE ( 'NONE', *, *, #25, .T. ) ;
#355 = CARTESIAN_POINT ( 'NONE',  ( 34.93420767782698988, 19.99999999999999645, -6.321724734770472587 ) ) ;
#356 = B_SPLINE_CURVE_WITH_KNOTS ( 'NONE', 3,
 ( #7684, #11748, #15744, #10079, #15575, #885, #3452, #9097, #3622, #16818, #9013, #14426, #12830, #2290, #14173, #621, #2110, #11499, #13092, #10426, #17157, #3713, #6274, #15486, #7510, #10172, #957, #3367, #2372, #8840, #14245, #8761, #2034, #12919, #15652, #11589, #16996, #4863, #6352, #3529, #14505, #8920, #11664, #8122, #3791, #2468, #11934, #9443, #9277, #16010 ),
 .UNSPECIFIED., .F., .F.,
 ( 4, 2, 2, 2, 2, 2, 2, 2, 2, 2, 2, 2, 2, 2, 2, 2, 2, 2, 2, 2, 2, 2, 2, 2, 4 ),
 ( 0.02172192739389855118, 0.02251948391625536658, 0.02331704043861218198, 0.02491215348332581278, 0.02650726652803944358, 0.02810237957275307438, 0.02969749261746670171, 0.03129260566218033252, 0.03209016218453714098, 0.03288771870689394250, 0.03328649696807235020, 0.03368527522925075790, 0.03448283175160756636, 0.03528038827396437482, 0.03567916653514278946, 0.03607794479632120410, 0.03687550131867804726, 0.03767305784103488348, 0.03847061436339171969, 0.03926817088574855591, 0.04086328393046227692, 0.04245839697517599792, 0.04405351001988971893, 0.04564862306460343994, 0.04724373610931716094 ),
 .UNSPECIFIED. ) ;
#357 = DIRECTION ( 'NONE',  ( 8.673617379884037937E-17, 0.000000000000000000, 1.000000000000000000 ) ) ;
#358 = EDGE_LOOP ( 'NONE', ( #12471, #2318, #7218, #8842 ) ) ;
#359 = CARTESIAN_POINT ( 'NONE',  ( -27.98221281347032274, 19.99999999999999645, 4.999999999999996447 ) ) ;
#360 = PRODUCT_RELATED_PRODUCT_CATEGORY ( 'part', '', ( #8716 ) ) ;
#361 = CYLINDRICAL_SURFACE ( 'NONE', #2522, 248.0000000000000000 ) ;
#362 = ORIENTED_EDGE ( 'NONE', *, *, #2234, .T. ) ;
#363 = CARTESIAN_POINT ( 'NONE',  ( 37.21337428997476593, 198.7412861714591941, -18.82352572523459600 ) ) ;
#364 = EDGE_CURVE ( 'NONE', #14743, #3326, #2669, .T. ) ;
#365 = CARTESIAN_POINT ( 'NONE',  ( -27.81025873171734375, 18.00000000000000355, 7.666431193274476641 ) ) ;
#366 = DIRECTION ( 'NONE',  ( -1.000000000000000000, -0.000000000000000000, -0.000000000000000000 ) ) ;
#367 = CARTESIAN_POINT ( 'NONE',  ( -206.3689767832464668, 174.5534660175772785, 3.987129972734268168 ) ) ;
#368 = DIRECTION ( 'NONE',  ( -1.000000000000000000, -0.000000000000000000, -0.000000000000000000 ) ) ;
#369 = CARTESIAN_POINT ( 'NONE',  ( -100.0000000000000000, 142.8100939375178200, -16.63501009223129756 ) ) ;
#370 = FACE_OUTER_BOUND ( 'NONE', #15719, .T. ) ;
#371 = ORIENTED_EDGE ( 'NONE', *, *, #3539, .F. ) ;
#372 = CARTESIAN_POINT ( 'NONE',  ( 24.48161681970857018, 138.6020828307752879, -11.64873334838780572 ) ) ;
#373 = EDGE_CURVE ( 'NONE', #8849, #8796, #6836, .T. ) ;
#374 = VERTEX_POINT ( 'NONE', #16306 ) ;
#375 = CARTESIAN_POINT ( 'NONE',  ( -68.00000000000000000, 171.6227766016838245, -19.49999999999999645 ) ) ;
#376 = CARTESIAN_POINT ( 'NONE',  ( -8.461393309425545795, 30.35704578695612099, -12.95687587100684368 ) ) ;
#377 = EDGE_LOOP ( 'NONE', ( #3921, #10271, #6852, #11471 ) ) ;
#378 = ORIENTED_EDGE ( 'NONE', *, *, #1221, .T. ) ;
#379 = LINE ( 'NONE', #5779, #16244 ) ;
#380 = CARTESIAN_POINT ( 'NONE',  ( 15.95607457770042181, 136.6882381644217048, 2.475222843549475638 ) ) ;
#381 = CARTESIAN_POINT ( 'NONE',  ( 13.38958197704232056, 130.3612470323695902, 12.52688079436099144 ) ) ;
#382 = ORIENTED_EDGE ( 'NONE', *, *, #10198, .F. ) ;
#383 = DIRECTION ( 'NONE',  ( 3.469446951953614189E-16, -1.000000000000000000, 0.000000000000000000 ) ) ;
#384 = LINE ( 'NONE', #14028, #11479 ) ;
#385 = CARTESIAN_POINT ( 'NONE',  ( -81.89019958151206424, 191.9899036175949618, 25.96511099662697930 ) ) ;
#386 = DIRECTION ( 'NONE',  ( 0.000000000000000000, 0.000000000000000000, 1.000000000000000000 ) ) ;
#387 = CARTESIAN_POINT ( 'NONE',  ( 17.50698843878764777, 29.94827730614627725, 12.57924512168886011 ) ) ;
#388 = DIRECTION ( 'NONE',  ( 0.000000000000000000, -0.4999999999999997224, 0.8660254037844387076 ) ) ;
#389 = EDGE_LOOP ( 'NONE', ( #662, #9822, #5339, #17357 ) ) ;
#390 = DIRECTION ( 'NONE',  ( 0.000000000000000000, 0.000000000000000000, 1.000000000000000000 ) ) ;
#391 = ADVANCED_FACE ( 'NONE', ( #9825 ), #19, .F. ) ;
#392 = ADVANCED_FACE ( 'NONE', ( #6907 ), #7804, .F. ) ;
#393 = DIRECTION ( 'NONE',  ( 1.000000000000000000, 0.000000000000000000, 0.000000000000000000 ) ) ;
#394 = EDGE_CURVE ( 'NONE', #12251, #2211, #12340, .T. ) ;
#395 = CARTESIAN_POINT ( 'NONE',  ( 27.15273249069231198, 19.99999999999999645, -20.88767039909325973 ) ) ;
#396 = CARTESIAN_POINT ( 'NONE',  ( -206.1506185320109239, 176.5415102007174255, 53.79077198841061147 ) ) ;
#397 = DIRECTION ( 'NONE',  ( -0.000000000000000000, -0.000000000000000000, 1.000000000000000000 ) ) ;
#398 = AXIS2_PLACEMENT_3D ( 'NONE', #9363, #2641, #5198 ) ;
#399 = VERTEX_POINT ( 'NONE', #184 ) ;
#400 = ORIENTED_EDGE ( 'NONE', *, *, #61, .T. ) ;
#401 = CARTESIAN_POINT ( 'NONE',  ( 8.997728150919979129, 132.8900016178789372, 12.55705910147062099 ) ) ;
#402 = EDGE_LOOP ( 'NONE', ( #8088, #12658, #10491, #2591 ) ) ;
#403 = EDGE_LOOP ( 'NONE', ( #5681, #2940, #16094, #11500 ) ) ;
#404 = CARTESIAN_POINT ( 'NONE',  ( 30.00000000000000355, 196.6227766016838245, 35.00200000000000244 ) ) ;
#405 = FACE_OUTER_BOUND ( 'NONE', #3645, .T. ) ;
#406 = CIRCLE ( 'NONE', #6632, 12.00000000000000000 ) ;
#407 = CARTESIAN_POINT ( 'NONE',  ( -96.00000000000001421, 201.6227766016838245, 0.000000000000000000 ) ) ;
#408 = CARTESIAN_POINT ( 'NONE',  ( -24.99999999999999289, 100.0000000000000142, -15.00000000000000000 ) ) ;
#409 = AXIS2_PLACEMENT_3D ( 'NONE', #3562, #17022, #2059 ) ;
#410 = CARTESIAN_POINT ( 'NONE',  ( 29.53214135918722505, 18.00000000000000000, -18.68621337607990185 ) ) ;
#411 = ORIENTED_EDGE ( 'NONE', *, *, #16163, .T. ) ;
#412 = CARTESIAN_POINT ( 'NONE',  ( 27.31119513844540947, 142.3932571782017931, 15.32207027268389510 ) ) ;
#413 = DIRECTION ( 'NONE',  ( 0.000000000000000000, 0.000000000000000000, 1.000000000000000000 ) ) ;
#414 = FACE_BOUND ( 'NONE', #1666, .T. ) ;
#415 = LINE ( 'NONE', #5821, #443 ) ;
#416 = AXIS2_PLACEMENT_3D ( 'NONE', #17010, #17352, #6371 ) ;
#417 = PLANE ( 'NONE',  #8765 ) ;
#418 = AXIS2_PLACEMENT_3D ( 'NONE', #14483, #7741, #8010 ) ;
#419 = ORIENTED_EDGE ( 'NONE', *, *, #3121, .F. ) ;
#420 = CARTESIAN_POINT ( 'NONE',  ( -50.00000000000000000, 191.6227766016837961, -1.224646799147353454E-15 ) ) ;
#421 = EDGE_LOOP ( 'NONE', ( #5552, #2069, #2676, #10202 ) ) ;
#422 = CARTESIAN_POINT ( 'NONE',  ( -75.17085894487867392, 193.0398713882428012, -27.68487141596273915 ) ) ;
#423 = CARTESIAN_POINT ( 'NONE',  ( 40.00000000000000711, 146.6227766016838245, 0.000000000000000000 ) ) ;
#424 = LINE ( 'NONE', #5834, #8946 ) ;
#425 = ADVANCED_FACE ( 'NONE', ( #5501 ), #4977, .T. ) ;
#426 = FACE_BOUND ( 'NONE', #13934, .T. ) ;
#427 = VECTOR ( 'NONE', #13768, 1000.000000000000000 ) ;
#428 = CARTESIAN_POINT ( 'NONE',  ( -95.00000000000000000, 171.6227766016838245, 0.000000000000000000 ) ) ;
#429 = DIRECTION ( 'NONE',  ( -0.000000000000000000, -0.000000000000000000, -1.000000000000000000 ) ) ;
#430 = MECHANICAL_DESIGN_GEOMETRIC_PRESENTATION_REPRESENTATION (  '', ( #7494 ), #12593 ) ;
#431 = CARTESIAN_POINT ( 'NONE',  ( -80.14161447679168759, 201.6221756766236979, 13.74903839801200789 ) ) ;
#432 = AXIS2_PLACEMENT_3D ( 'NONE', #5586, #6655, #5500 ) ;
#433 = FACE_BOUND ( 'NONE', #13642, .T. ) ;
#434 = ORIENTED_EDGE ( 'NONE', *, *, #16551, .T. ) ;
#435 = EDGE_LOOP ( 'NONE', ( #4715, #8702, #12659, #943, #16358, #4658 ) ) ;
#436 = CARTESIAN_POINT ( 'NONE',  ( 24.40970717605596718, 29.87515913883691354, -8.215055496182330330 ) ) ;
#437 = CARTESIAN_POINT ( 'NONE',  ( 27.04079503965286690, 139.2301514590222098, -6.313402927548398047 ) ) ;
#438 = ORIENTED_EDGE ( 'NONE', *, *, #11422, .T. ) ;
#439 = CARTESIAN_POINT ( 'NONE',  ( -14.83003349241583813, 19.99999999999883116, 8.298189366023557056 ) ) ;
#440 = DIRECTION ( 'NONE',  ( -1.000000000000000000, 0.000000000000000000, 0.000000000000000000 ) ) ;
#441 = VECTOR ( 'NONE', #9945, 1000.000000000000000 ) ;
#442 = ORIENTED_EDGE ( 'NONE', *, *, #11491, .T. ) ;
#443 = VECTOR ( 'NONE', #15203, 1000.000000000000000 ) ;
#444 = DIRECTION ( 'NONE',  ( -1.000000000000000000, -0.000000000000000000, -0.000000000000000000 ) ) ;
#445 = CARTESIAN_POINT ( 'NONE',  ( -27.94760966554430937, 18.00000000000000355, 6.338314452217974626 ) ) ;
#446 = EDGE_CURVE ( 'NONE', #9960, #12327, #12060, .T. ) ;
#447 = DIRECTION ( 'NONE',  ( -0.000000000000000000, -0.000000000000000000, -1.000000000000000000 ) ) ;
#448 = CARTESIAN_POINT ( 'NONE',  ( -207.5170152892447959, 175.0764231502095072, 3.989746324742934558 ) ) ;
#449 = PLANE ( 'NONE',  #5426 ) ;
#450 = CARTESIAN_POINT ( 'NONE',  ( -32.02886766642249228, 119.9418479153533781, 5.500000000000000888 ) ) ;
#451 = CARTESIAN_POINT ( 'NONE',  ( -74.40218896425085404, 141.6107120069882512, -13.74530841833676220 ) ) ;
#452 = AXIS2_PLACEMENT_3D ( 'NONE', #1785, #447, #9743 ) ;
#453 = VERTEX_POINT ( 'NONE', #5588 ) ;
#454 = DIRECTION ( 'NONE',  ( 1.000000000000000000, -0.000000000000000000, -0.000000000000000000 ) ) ;
#455 = EDGE_CURVE ( 'NONE', #7796, #10705, #11208, .T. ) ;
#456 = AXIS2_PLACEMENT_3D ( 'NONE', #11979, #6311, #7995 ) ;
#457 = VERTEX_POINT ( 'NONE', #10979 ) ;
#458 = EDGE_CURVE ( 'NONE', #11543, #11435, #15731, .T. ) ;
#459 = CARTESIAN_POINT ( 'NONE',  ( -95.00000000000000000, 171.6227766016838245, 0.000000000000000000 ) ) ;
#460 = EDGE_CURVE ( 'NONE', #8505, #14597, #2443, .T. ) ;
#461 = DIRECTION ( 'NONE',  ( -0.000000000000000000, -0.000000000000000000, -1.000000000000000000 ) ) ;
#462 = ORIENTED_EDGE ( 'NONE', *, *, #5545, .F. ) ;
#463 = DIRECTION ( 'NONE',  ( 1.000000000000000000, 0.000000000000000000, 0.000000000000000000 ) ) ;
#464 = CYLINDRICAL_SURFACE ( 'NONE', #1410, 2.499999999999998668 ) ;
#465 = CARTESIAN_POINT ( 'NONE',  ( 24.34257225596279639, 138.6622241066778543, 11.80661878326775494 ) ) ;
#466 = VECTOR ( 'NONE', #9041, 1000.000000000000000 ) ;
#467 = AXIS2_PLACEMENT_3D ( 'NONE', #16027, #3907, #7967 ) ;
#468 = ORIENTED_EDGE ( 'NONE', *, *, #15742, .T. ) ;
#469 = ITEM_DEFINED_TRANSFORMATION ( 'NONE', 'NONE', #8959,  #3583 ) ;
#470 = ADVANCED_FACE ( 'NONE', ( #12227 ), #3105, .T. ) ;
#471 = LINE ( 'NONE', #14027, #16068 ) ;
#472 = VECTOR ( 'NONE', #10118, 1000.000000000000114 ) ;
#473 = PRESENTATION_LAYER_ASSIGNMENT (  '', '', ( #2461 ) ) ;
#474 = DIRECTION ( 'NONE',  ( -1.000000000000000000, 0.000000000000000000, 0.000000000000000000 ) ) ;
#475 = AXIS2_PLACEMENT_3D ( 'NONE', #11596, #1866, #6196 ) ;
#476 = CARTESIAN_POINT ( 'NONE',  ( -78.09342651567857274, 191.9854139975492160, 25.96938468333279104 ) ) ;
#477 = DIRECTION ( 'NONE',  ( -1.000000000000000000, -0.000000000000000000, -0.000000000000000000 ) ) ;
#478 = CARTESIAN_POINT ( 'NONE',  ( 19.81659905433974700, 29.90262535319825332, 11.35915249282563444 ) ) ;
#479 = CARTESIAN_POINT ( 'NONE',  ( -7.379000772444995526, 30.00000000000000000, -13.00000000000000178 ) ) ;
#480 = ORIENTED_EDGE ( 'NONE', *, *, #11200, .F. ) ;
#481 = DIRECTION ( 'NONE',  ( 0.000000000000000000, 1.000000000000000000, 0.000000000000000000 ) ) ;
#482 = CARTESIAN_POINT ( 'NONE',  ( 2.370000000000000551, -4.750000000000000888, -5.817072295949928412E-16 ) ) ;
#483 = CARTESIAN_POINT ( 'NONE',  ( 32.91012024024373517, 19.99999999999999289, -13.86436652238006673 ) ) ;
#484 = DIRECTION ( 'NONE',  ( -1.000000000000000000, 0.000000000000000000, 0.000000000000000000 ) ) ;
#485 = CARTESIAN_POINT ( 'NONE',  ( -50.00000000000000000, 171.6227766016838245, 0.000000000000000000 ) ) ;
#486 = ORIENTED_EDGE ( 'NONE', *, *, #6340, .F. ) ;
#487 = AXIS2_PLACEMENT_3D ( 'NONE', #11537, #16029, #3909 ) ;
#488 = ORIENTED_EDGE ( 'NONE', *, *, #9995, .F. ) ;
#489 = VERTEX_POINT ( 'NONE', #13915 ) ;
#490 = ORIENTED_EDGE ( 'NONE', *, *, #17231, .F. ) ;
#491 = CIRCLE ( 'NONE', #16041, 33.00000000000000000 ) ;
#492 = CYLINDRICAL_SURFACE ( 'NONE', #1416, 10.00000000000000178 ) ;
#493 = ORIENTED_EDGE ( 'NONE', *, *, #9337, .F. ) ;
#494 = CARTESIAN_POINT ( 'NONE',  ( 40.00000000000000711, 171.6227766016838245, 0.000000000000000000 ) ) ;
#495 = EDGE_LOOP ( 'NONE', ( #13630, #14725, #1232, #7431, #16585, #10286, #6595, #15301, #1355, #7450, #11318, #10338 ) ) ;
#496 = EDGE_CURVE ( 'NONE', #16329, #13265, #6750, .T. ) ;
#497 = EDGE_CURVE ( 'NONE', #6006, #5256, #4292, .T. ) ;
#498 = DIRECTION ( 'NONE',  ( -1.000000000000000000, -0.000000000000000000, 0.000000000000000000 ) ) ;
#499 = EDGE_CURVE ( 'NONE', #9593, #12318, #8101, .T. ) ;
#500 = CIRCLE ( 'NONE', #10943, 10.00000000000000178 ) ;
#501 = CARTESIAN_POINT ( 'NONE',  ( 40.00000000000000711, 204.6227766016838245, -2.020667218593133100E-15 ) ) ;
#502 = DIRECTION ( 'NONE',  ( -1.000000000000000000, 0.000000000000000000, 0.000000000000000000 ) ) ;
#503 = CARTESIAN_POINT ( 'NONE',  ( -45.00000000000000000, 130.0000000000000000, -15.00000000000000000 ) ) ;
#504 = AXIS2_PLACEMENT_3D ( 'NONE', #14770, #8028, #16194 ) ;
#505 = AXIS2_PLACEMENT_3D ( 'NONE', #14744, #2617, #15707 ) ;
#506 = VECTOR ( 'NONE', #763, 1000.000000000000000 ) ;
#507 = ORIENTED_EDGE ( 'NONE', *, *, #5137, .F. ) ;
#508 = DIRECTION ( 'NONE',  ( -1.000000000000000000, -0.000000000000000000, -0.000000000000000000 ) ) ;
#509 = CARTESIAN_POINT ( 'NONE',  ( -192.9999999999999716, 171.6227766016838245, 0.000000000000000000 ) ) ;
#510 = DIRECTION ( 'NONE',  ( -1.000000000000000000, 0.000000000000000000, 0.000000000000000000 ) ) ;
#511 = CARTESIAN_POINT ( 'NONE',  ( -8.766611209710754693, 19.99999999999771916, -14.60748648876205458 ) ) ;
#512 = LINE ( 'NONE', #4502, #12581 ) ;
#513 = PRODUCT_DEFINITION_SHAPE ( 'NONE', 'NONE',  #17523 ) ;
#514 = CYLINDRICAL_SURFACE ( 'NONE', #16412, 6.000000000000005329 ) ;
#515 = CIRCLE ( 'NONE', #6739, 8.000000000000000000 ) ;
#516 = ORIENTED_EDGE ( 'NONE', *, *, #7943, .F. ) ;
#517 = CARTESIAN_POINT ( 'NONE',  ( -75.00000000000002842, 146.6227766016838245, 0.000000000000000000 ) ) ;
#518 = CIRCLE ( 'NONE', #8724, 4.000000000000001776 ) ;
#519 = ORIENTED_EDGE ( 'NONE', *, *, #4625, .F. ) ;
#520 = EDGE_CURVE ( 'NONE', #7447, #15746, #3010, .T. ) ;
#521 = FILL_AREA_STYLE_COLOUR ( '', #2206 ) ;
#522 = ADVANCED_FACE ( 'NONE', ( #13830 ), #1695, .F. ) ;
#523 = DIRECTION ( 'NONE',  ( 1.000000000000000000, 0.000000000000000000, 0.000000000000000000 ) ) ;
#524 = EDGE_LOOP ( 'NONE', ( #9216, #14969 ) ) ;
#525 = CARTESIAN_POINT ( 'NONE',  ( -725.0000000000000000, 30.00000000000000000, -25.00000000000000000 ) ) ;
#526 = CARTESIAN_POINT ( 'NONE',  ( 39.99999999999998579, 4.000000000000000000, -33.00000000000000000 ) ) ;
#527 = DIRECTION ( 'NONE',  ( 1.000000000000000000, -0.000000000000000000, -0.000000000000000000 ) ) ;
#528 = ORIENTED_EDGE ( 'NONE', *, *, #5545, .T. ) ;
#529 = CARTESIAN_POINT ( 'NONE',  ( 27.99999999999998224, 9.999999999999998224, 0.000000000000000000 ) ) ;
#530 = CARTESIAN_POINT ( 'NONE',  ( -77.50000000000001421, 196.6227766016838245, 10.00000000000000178 ) ) ;
#531 = AXIS2_PLACEMENT_3D ( 'NONE', #7704, #6212, #3646 ) ;
#532 = CARTESIAN_POINT ( 'NONE',  ( -79.43217333917553447, 201.5917424073650182, 13.81529814621275953 ) ) ;
#533 = CIRCLE ( 'NONE', #811, 21.61734737250326077 ) ;
#534 = SURFACE_STYLE_USAGE ( .BOTH. , #5674 ) ;
#535 = EDGE_LOOP ( 'NONE', ( #5840, #7471, #16377, #3579 ) ) ;
#536 = ORIENTED_EDGE ( 'NONE', *, *, #1514, .F. ) ;
#537 = CARTESIAN_POINT ( 'NONE',  ( 24.72170379509201865, 19.99999999999999645, -7.619165077982883894 ) ) ;
#538 = CARTESIAN_POINT ( 'NONE',  ( 19.59022622986824302, 142.1737554346910599, -14.89790021284453303 ) ) ;
#539 = VERTEX_POINT ( 'NONE', #274 ) ;
#540 = ADVANCED_FACE ( 'NONE', ( #12491 ), #2116, .T. ) ;
#541 = CARTESIAN_POINT ( 'NONE',  ( 35.00000000000000711, 146.6227766016838245, 35.00200000000000244 ) ) ;
#542 = CARTESIAN_POINT ( 'NONE',  ( -187.6513770290094385, 171.1853623553244006, 0.7576236986490064718 ) ) ;
#543 = AXIS2_PLACEMENT_3D ( 'NONE', #9206, #16030, #16296 ) ;
#544 = VERTEX_POINT ( 'NONE', #5945 ) ;
#545 = AXIS2_PLACEMENT_3D ( 'NONE', #15355, #5797, #5891 ) ;
#546 = PLANE ( 'NONE',  #7342 ) ;
#547 = AXIS2_PLACEMENT_3D ( 'NONE', #310, #15173, #4211 ) ;
#548 = CARTESIAN_POINT ( 'NONE',  ( -22.79696676584440596, 18.00000000000000711, 18.34105320469107170 ) ) ;
#549 = CYLINDRICAL_SURFACE ( 'NONE', #11760, 35.00000000000000000 ) ;
#550 = DIRECTION ( 'NONE',  ( 0.000000000000000000, 0.000000000000000000, 1.000000000000000000 ) ) ;
#551 = CARTESIAN_POINT ( 'NONE',  ( -7.379000772444995526, 18.00000000000000355, 12.99999999999999822 ) ) ;
#552 = DIRECTION ( 'NONE',  ( 1.000000000000000000, 0.000000000000000000, 0.000000000000000000 ) ) ;
#553 = CARTESIAN_POINT ( 'NONE',  ( -72.50000000000002842, 146.6227766016838245, -21.54065922853802562 ) ) ;
#554 = VERTEX_POINT ( 'NONE', #15318 ) ;
#555 = CYLINDRICAL_SURFACE ( 'NONE', #8157, 33.00000000000000000 ) ;
#556 = AXIS2_PLACEMENT_3D ( 'NONE', #15496, #7518, #2210 ) ;
#557 = VECTOR ( 'NONE', #9968, 1000.000000000000114 ) ;
#558 = AXIS2_PLACEMENT_3D ( 'NONE', #9560, #17361, #13561 ) ;
#559 = ORIENTED_EDGE ( 'NONE', *, *, #15927, .T. ) ;
#560 = CARTESIAN_POINT ( 'NONE',  ( -90.80384757729339640, 204.6227766016838245, 0.000000000000000000 ) ) ;
#561 = VECTOR ( 'NONE', #2674, 1000.000000000000000 ) ;
#562 = CARTESIAN_POINT ( 'NONE',  ( -26.10410744458347665, 18.00000000000000000, -13.37721135299797304 ) ) ;
#563 = ORIENTED_EDGE ( 'NONE', *, *, #11755, .F. ) ;
#564 = EDGE_CURVE ( 'NONE', #4853, #5097, #11488, .T. ) ;
#565 = CARTESIAN_POINT ( 'NONE',  ( 23.79315516583586643, 19.99999999999999645, 22.94240041036162836 ) ) ;
#566 = DIRECTION ( 'NONE',  ( 0.000000000000000000, 0.000000000000000000, -1.000000000000000000 ) ) ;
#567 = CARTESIAN_POINT ( 'NONE',  ( 15.80099858973940030, 127.9994182179736413, 10.08996921773076316 ) ) ;
#568 = AXIS2_PLACEMENT_3D ( 'NONE', #14760, #4313, #60 ) ;
#569 = AXIS2_PLACEMENT_3D ( 'NONE', #5580, #6650, #6830 ) ;
#570 = VERTEX_POINT ( 'NONE', #6023 ) ;
#571 = CARTESIAN_POINT ( 'NONE',  ( 37.99999999999999289, 2.000000000000000000, -8.789265611615818404E-15 ) ) ;
#572 = EDGE_CURVE ( 'NONE', #3368, #13835, #6120, .T. ) ;
#573 = CIRCLE ( 'NONE', #11580, 2.500000000000000444 ) ;
#574 = DIRECTION ( 'NONE',  ( 0.000000000000000000, 1.000000000000000000, 0.000000000000000000 ) ) ;
#575 = EDGE_CURVE ( 'NONE', #8346, #5702, #12911, .T. ) ;
#576 = DIRECTION ( 'NONE',  ( 0.000000000000000000, 0.000000000000000000, 1.000000000000000000 ) ) ;
#577 = DIRECTION ( 'NONE',  ( -1.000000000000000000, 1.040834085586084059E-15, 0.000000000000000000 ) ) ;
#578 = CARTESIAN_POINT ( 'NONE',  ( 17.01529014380724192, 17.99999999999942801, 12.76845467807931733 ) ) ;
#579 = CARTESIAN_POINT ( 'NONE',  ( -68.00000000000000000, 204.6227766016838245, 0.000000000000000000 ) ) ;
#580 = ORIENTED_EDGE ( 'NONE', *, *, #7866, .T. ) ;
#581 = CARTESIAN_POINT ( 'NONE',  ( -725.0000000000000000, 30.00000000000000000, 13.00000000000000000 ) ) ;
#582 = CARTESIAN_POINT ( 'NONE',  ( 225.0000000000000000, 89.99999999999997158, 4.999999999999999112 ) ) ;
#583 = VERTEX_POINT ( 'NONE', #4786 ) ;
#584 = DIRECTION ( 'NONE',  ( 0.000000000000000000, 0.000000000000000000, 1.000000000000000000 ) ) ;
#585 = CARTESIAN_POINT ( 'NONE',  ( -45.00000000000000000, 122.0000000000000142, -4.999999999999999112 ) ) ;
#586 = AXIS2_PLACEMENT_3D ( 'NONE', #156, #1313, #13701 ) ;
#587 = ORIENTED_EDGE ( 'NONE', *, *, #6448, .T. ) ;
#588 = VERTEX_POINT ( 'NONE', #3277 ) ;
#589 = ORIENTED_EDGE ( 'NONE', *, *, #4843, .T. ) ;
#590 = VECTOR ( 'NONE', #14056, 1000.000000000000000 ) ;
#591 = CARTESIAN_POINT ( 'NONE',  ( 11.63249183333955017, 139.6944596454877114, 10.84829254633709184 ) ) ;
#592 = ORIENTED_EDGE ( 'NONE', *, *, #11333, .F. ) ;
#593 = DIRECTION ( 'NONE',  ( 1.000000000000000000, 0.000000000000000000, 0.000000000000000000 ) ) ;
#594 = ORIENTED_EDGE ( 'NONE', *, *, #13777, .F. ) ;
#595 = SURFACE_STYLE_FILL_AREA ( #3338 ) ;
#596 = DIRECTION ( 'NONE',  ( 1.000000000000000000, 0.000000000000000000, 0.000000000000000000 ) ) ;
#597 = CARTESIAN_POINT ( 'NONE',  ( 13.91851620013868995, 127.9827558526829563, 9.294367823883964874 ) ) ;
#598 = DIRECTION ( 'NONE',  ( 0.000000000000000000, 1.000000000000000000, 0.000000000000000000 ) ) ;
#599 = AXIS2_PLACEMENT_3D ( 'NONE', #14005, #3199, #15140 ) ;
#600 = CARTESIAN_POINT ( 'NONE',  ( 25.00000000000000711, 146.6227766016838245, -12.99999999999999822 ) ) ;
#601 = B_SPLINE_CURVE_WITH_KNOTS ( 'NONE', 3,
 ( #15955, #13311, #9052, #1176 ),
 .UNSPECIFIED., .F., .F.,
 ( 4, 4 ),
 ( -6.324563032106999871E-06, 0.0003067249959486805411 ),
 .UNSPECIFIED. ) ;
#602 = ORIENTED_EDGE ( 'NONE', *, *, #14098, .F. ) ;
#603 = FACE_OUTER_BOUND ( 'NONE', #10174, .T. ) ;
#604 = LINE ( 'NONE', #8649, #6198 ) ;
#605 = PLANE ( 'NONE',  #3116 ) ;
#606 = CARTESIAN_POINT ( 'NONE',  ( -8.792264229871568304, 30.31966024794114745, -14.93731107458715357 ) ) ;
#607 = EDGE_CURVE ( 'NONE', #15092, #6530, #17001, .T. ) ;
#608 = AXIS2_PLACEMENT_3D ( 'NONE', #6490, #13127, #6395 ) ;
#609 = FACE_OUTER_BOUND ( 'NONE', #3195, .T. ) ;
#610 = ORIENTED_EDGE ( 'NONE', *, *, #4593, .T. ) ;
#611 = LINE ( 'NONE', #16893, #6704 ) ;
#612 = EDGE_CURVE ( 'NONE', #8809, #13930, #10178, .T. ) ;
#613 = EDGE_LOOP ( 'NONE', ( #6152, #6292 ) ) ;
#614 = CARTESIAN_POINT ( 'NONE',  ( -85.77828040291200296, 194.9977432358044496, -26.05112671349591125 ) ) ;
#615 = DIRECTION ( 'NONE',  ( 0.000000000000000000, 1.000000000000000000, 0.000000000000000000 ) ) ;
#616 = DIRECTION ( 'NONE',  ( 0.000000000000000000, 0.000000000000000000, 1.000000000000000000 ) ) ;
#617 = ORIENTED_EDGE ( 'NONE', *, *, #4810, .T. ) ;
#618 = DIRECTION ( 'NONE',  ( 0.000000000000000000, 0.000000000000000000, -1.000000000000000000 ) ) ;
#619 = CYLINDRICAL_SURFACE ( 'NONE', #11277, 6.000000000000005329 ) ;
#620 = CARTESIAN_POINT ( 'NONE',  ( -80.49255897422042949, 201.5998317580112200, 13.79770299781518972 ) ) ;
#621 = CARTESIAN_POINT ( 'NONE',  ( 27.40877793924366301, 202.0384121146825578, -17.31838511551978144 ) ) ;
#622 = ORIENTED_EDGE ( 'NONE', *, *, #10511, .F. ) ;
#623 = EDGE_CURVE ( 'NONE', #8295, #4586, #6392, .T. ) ;
#624 = EDGE_CURVE ( 'NONE', #1718, #6006, #5357, .T. ) ;
#625 = EDGE_CURVE ( 'NONE', #4234, #16058, #12632, .T. ) ;
#626 = ORIENTED_EDGE ( 'NONE', *, *, #13035, .T. ) ;
#627 = CARTESIAN_POINT ( 'NONE',  ( 30.00000000000001066, 146.6227766016838245, -35.00200000000000244 ) ) ;
#628 = EDGE_CURVE ( 'NONE', #9656, #12025, #15580, .T. ) ;
#629 = LINE ( 'NONE', #6194, #9795 ) ;
#630 = ORIENTED_EDGE ( 'NONE', *, *, #2454, .F. ) ;
#631 = DIRECTION ( 'NONE',  ( 0.000000000000000000, 0.000000000000000000, -1.000000000000000000 ) ) ;
#632 = CARTESIAN_POINT ( 'NONE',  ( 7.290380404777190293, 133.8591131982526008, -12.94327073059132971 ) ) ;
#633 = ORIENTED_EDGE ( 'NONE', *, *, #12413, .F. ) ;
#634 = CARTESIAN_POINT ( 'NONE',  ( -27.98221281347037959, 20.00000000000000000, 4.999999999999999112 ) ) ;
#635 = UNCERTAINTY_MEASURE_WITH_UNIT (LENGTH_MEASURE( 1.000000000000000082E-05 ), #4493, 'distance_accuracy_value', 'NONE');
#636 = CARTESIAN_POINT ( 'NONE',  ( -68.00000000000000000, 171.6227766016838245, 0.000000000000000000 ) ) ;
#637 = CARTESIAN_POINT ( 'NONE',  ( -207.6770884633517085, 166.3723159270569738, -1.150078995496658596 ) ) ;
#638 = CARTESIAN_POINT ( 'NONE',  ( -207.7508999721942189, 175.3364228813296108, 3.959069933371625716 ) ) ;
#639 = CARTESIAN_POINT ( 'NONE',  ( -12.55890155933014363, 17.99999999999884182, 7.515612101507582743 ) ) ;
#640 = LINE ( 'NONE', #12678, #3519 ) ;
#641 = CARTESIAN_POINT ( 'NONE',  ( -153.0000000000000284, 171.6227766016838245, 0.000000000000000000 ) ) ;
#642 = ORIENTED_EDGE ( 'NONE', *, *, #1514, .T. ) ;
#643 = FACE_OUTER_BOUND ( 'NONE', #1205, .T. ) ;
#644 = ORIENTED_EDGE ( 'NONE', *, *, #1969, .F. ) ;
#645 = CARTESIAN_POINT ( 'NONE',  ( 27.75000000000000000, 0.000000000000000000, 0.000000000000000000 ) ) ;
#646 = DIRECTION ( 'NONE',  ( 0.000000000000000000, 0.000000000000000000, 1.000000000000000000 ) ) ;
#647 = VERTEX_POINT ( 'NONE', #3540 ) ;
#648 = DIRECTION ( 'NONE',  ( 8.673617379884037937E-17, -2.891205793294676354E-16, -1.000000000000000000 ) ) ;
#649 = CARTESIAN_POINT ( 'NONE',  ( 24.93507336697333798, 29.86842105264641845, 5.660862367392566874 ) ) ;
#650 = CARTESIAN_POINT ( 'NONE',  ( 14.18611645313626290, 129.6406627243902676, 11.87032202561248617 ) ) ;
#651 = ORIENTED_EDGE ( 'NONE', *, *, #1422, .F. ) ;
#652 = ITEM_DEFINED_TRANSFORMATION ( 'NONE', 'NONE', #14353,  #3583 ) ;
#653 = DIRECTION ( 'NONE',  ( -1.000000000000000000, -0.000000000000000000, -0.000000000000000000 ) ) ;
#654 = DIRECTION ( 'NONE',  ( -1.000000000000000000, 0.000000000000000000, 0.000000000000000000 ) ) ;
#655 = CARTESIAN_POINT ( 'NONE',  ( -75.10425368493336862, 195.5720014495396981, 22.70655749026625614 ) ) ;
#656 = CYLINDRICAL_SURFACE ( 'NONE', #15299, 1.000000000000000888 ) ;
#657 =( REPRESENTATION_RELATIONSHIP ('NONE','NONE', #9723, #6585 ) REPRESENTATION_RELATIONSHIP_WITH_TRANSFORMATION ( #7289 )SHAPE_REPRESENTATION_RELATIONSHIP( ) );
#658 = EDGE_CURVE ( 'NONE', #1654, #17318, #629, .T. ) ;
#659 = CARTESIAN_POINT ( 'NONE',  ( 1.559999999999998943, 1.299038105676664223, 0.7500000000000006661 ) ) ;
#660 = DIRECTION ( 'NONE',  ( 0.8571673013836867971, 1.049727191973306626E-16, -0.5150380737757237481 ) ) ;
#661 = EDGE_CURVE ( 'NONE', #8817, #10086, #2457, .T. ) ;
#662 = ORIENTED_EDGE ( 'NONE', *, *, #10245, .F. ) ;
#663 = DIRECTION ( 'NONE',  ( 1.000000000000000000, 0.000000000000000000, -0.000000000000000000 ) ) ;
#664 = CARTESIAN_POINT ( 'NONE',  ( -206.3689767832464668, 174.5534660175772785, 53.79077198841061147 ) ) ;
#665 = EDGE_LOOP ( 'NONE', ( #2497, #10383, #12994, #3390 ) ) ;
#666 = CARTESIAN_POINT ( 'NONE',  ( 39.99999999999998579, 4.000000000000000000, -33.00000000000000000 ) ) ;
#667 = DIRECTION ( 'NONE',  ( -1.000000000000000000, 0.000000000000000000, 0.000000000000000000 ) ) ;
#668 = VERTEX_POINT ( 'NONE', #6105 ) ;
#669 = ORIENTED_EDGE ( 'NONE', *, *, #10810, .F. ) ;
#670 = ORIENTED_EDGE ( 'NONE', *, *, #4740, .F. ) ;
#671 = EDGE_CURVE ( 'NONE', #11068, #15447, #12662, .T. ) ;
#672 = ORIENTED_EDGE ( 'NONE', *, *, #16461, .F. ) ;
#673 = LINE ( 'NONE', #4749, #14088 ) ;
#674 = EDGE_LOOP ( 'NONE', ( #1760, #15151, #9125, #15624 ) ) ;
#675 = SHAPE_REPRESENTATION_RELATIONSHIP ( 'NONE' , 'NONE' ,  #10772, #1721 ) ;
#676 = DIRECTION ( 'NONE',  ( 0.000000000000000000, 1.000000000000000000, 0.000000000000000000 ) ) ;
#677 = CARTESIAN_POINT ( 'NONE',  ( 11.61330907248435018, 130.6704317944142986, 11.35602788888950698 ) ) ;
#678 = CARTESIAN_POINT ( 'NONE',  ( 0.000000000000000000, -2.375000000000000000, -4.362804221962446556E-16 ) ) ;
#679 = CARTESIAN_POINT ( 'NONE',  ( 37.50000000000000711, 146.0561595177564129, -20.88304578468306261 ) ) ;
#680 = EDGE_CURVE ( 'NONE', #399, #15865, #9191, .T. ) ;
#681 = EDGE_LOOP ( 'NONE', ( #12915, #11101, #10298, #13282 ) ) ;
#682 = CARTESIAN_POINT ( 'NONE',  ( 32.67951861369070343, 142.3872899932706844, 15.31067380954020862 ) ) ;
#683 = CARTESIAN_POINT ( 'NONE',  ( 17.58250999373992585, 125.2198453306090329, 1.325401613797208934E-14 ) ) ;
#684 = CARTESIAN_POINT ( 'NONE',  ( -80.00000000000002842, 146.6227766016838245, -16.00000000000000000 ) ) ;
#685 = CARTESIAN_POINT ( 'NONE',  ( -13.51825462539708056, 19.99999999999884892, -10.94502331224290259 ) ) ;
#686 =( NAMED_UNIT ( * ) SI_UNIT ( $, .STERADIAN. ) SOLID_ANGLE_UNIT ( ) );
#687 = EDGE_CURVE ( 'NONE', #15915, #10010, #12076, .T. ) ;
#688 = ADVANCED_FACE ( 'NONE', ( #5209 ), #12027, .F. ) ;
#689 = ADVANCED_FACE ( 'NONE', ( #14335 ), #14508, .T. ) ;
#690 = SHAPE_REPRESENTATION ( 'Keyless Chuck', ( #3583 ), #12675 ) ;
#691 = CARTESIAN_POINT ( 'NONE',  ( -103.0000000000000142, 171.6227766016838245, 0.000000000000000000 ) ) ;
#692 = ORIENTED_EDGE ( 'NONE', *, *, #13103, .T. ) ;
#693 = CARTESIAN_POINT ( 'NONE',  ( 196.0000000000000000, 175.6227766016838245, 8.071800142134975431 ) ) ;
#694 = CIRCLE ( 'NONE', #3507, 4.750000000000000000 ) ;
#695 = ORIENTED_EDGE ( 'NONE', *, *, #11443, .F. ) ;
#696 =( LENGTH_UNIT ( ) NAMED_UNIT ( * ) SI_UNIT ( .MILLI., .METRE. ) );
#697 = CARTESIAN_POINT ( 'NONE',  ( -85.89524066039361117, 195.4942584061382149, -25.59693137756977421 ) ) ;
#698 = AXIS2_PLACEMENT_3D ( 'NONE', #16846, #8791, #6045 ) ;
#699 = DIRECTION ( 'NONE',  ( 0.000000000000000000, 0.000000000000000000, -1.000000000000000000 ) ) ;
#700 = EDGE_CURVE ( 'NONE', #11501, #8340, #15923, .T. ) ;
#701 = CARTESIAN_POINT ( 'NONE',  ( 15.53715976346056493, 125.3980538582347748, -5.670872899454017180 ) ) ;
#702 = ORIENTED_EDGE ( 'NONE', *, *, #13472, .T. ) ;
#703 = FACE_OUTER_BOUND ( 'NONE', #16932, .T. ) ;
#704 = DIRECTION ( 'NONE',  ( 0.000000000000000000, 0.000000000000000000, -1.000000000000000000 ) ) ;
#705 = CARTESIAN_POINT ( 'NONE',  ( -75.98683855290481404, 199.6193856840139631, 17.47499078086475777 ) ) ;
#706 = CARTESIAN_POINT ( 'NONE',  ( 50.00000000000000000, 171.6227766016838245, 0.000000000000000000 ) ) ;
#707 = VECTOR ( 'NONE', #1161, 1000.000000000000000 ) ;
#708 = ORIENTED_EDGE ( 'NONE', *, *, #14469, .F. ) ;
#709 = VECTOR ( 'NONE', #13927, 1000.000000000000000 ) ;
#710 = ORIENTED_EDGE ( 'NONE', *, *, #6159, .T. ) ;
#711 = CARTESIAN_POINT ( 'NONE',  ( 24.93034343272635667, 19.99999999999999645, -22.33460256652156062 ) ) ;
#712 = DIRECTION ( 'NONE',  ( -0.8571673013836867971, 0.000000000000000000, -0.5150380737757237481 ) ) ;
#713 = VERTEX_POINT ( 'NONE', #3894 ) ;
#714 = DIRECTION ( 'NONE',  ( 0.000000000000000000, 0.000000000000000000, -1.000000000000000000 ) ) ;
#715 = DIRECTION ( 'NONE',  ( -0.000000000000000000, -0.000000000000000000, -1.000000000000000000 ) ) ;
#716 = EDGE_LOOP ( 'NONE', ( #4936, #15212, #7223, #17300 ) ) ;
#717 = FACE_BOUND ( 'NONE', #9395, .T. ) ;
#718 = CIRCLE ( 'NONE', #10601, 249.9999999999999716 ) ;
#719 = EDGE_CURVE ( 'NONE', #2134, #4864, #6633, .T. ) ;
#720 = EDGE_CURVE ( 'NONE', #16285, #7408, #500, .T. ) ;
#721 = ADVANCED_FACE ( 'NONE', ( #6455 ), #11074, .F. ) ;
#722 = VECTOR ( 'NONE', #15291, 1000.000000000000000 ) ;
#723 = CARTESIAN_POINT ( 'NONE',  ( 48.00000000000000000, 171.6227766016838245, 10.00000337241048953 ) ) ;
#724 = CARTESIAN_POINT ( 'NONE',  ( -102.0000000000000142, 201.6227766016838245, 0.000000000000000000 ) ) ;
#725 = CARTESIAN_POINT ( 'NONE',  ( -9.392228533940972568, 30.65825049985634010, 12.80200153553487752 ) ) ;
#726 = CARTESIAN_POINT ( 'NONE',  ( 40.00000000000000711, 206.6227766016838245, 0.000000000000000000 ) ) ;
#727 = CARTESIAN_POINT ( 'NONE',  ( 30.13973646015553243, 140.6228917578588948, -16.24829651775490902 ) ) ;
#728 = ORIENTED_EDGE ( 'NONE', *, *, #8884, .T. ) ;
#729 = LINE ( 'NONE', #14192, #7026 ) ;
#730 = VERTEX_POINT ( 'NONE', #10789 ) ;
#731 = DIRECTION ( 'NONE',  ( 0.000000000000000000, 0.000000000000000000, 1.000000000000000000 ) ) ;
#732 = VECTOR ( 'NONE', #9698, 1000.000000000000000 ) ;
#733 = CARTESIAN_POINT ( 'NONE',  ( -32.64269715136552463, 118.7804878048780779, 4.500000000000000000 ) ) ;
#734 = CIRCLE ( 'NONE', #12313, 12.00000000000000000 ) ;
#735 = VERTEX_POINT ( 'NONE', #16202 ) ;
#736 = CARTESIAN_POINT ( 'NONE',  ( 20.13757169487763576, 19.99999999999999289, 24.32197800972832624 ) ) ;
#737 = AXIS2_PLACEMENT_3D ( 'NONE', #15583, #12931, #3375 ) ;
#738 = CARTESIAN_POINT ( 'NONE',  ( 19.35452547490215736, 29.94096051140668280, 13.97567760708249551 ) ) ;
#739 = CARTESIAN_POINT ( 'NONE',  ( -195.2299705378136991, 173.3300053194287784, 3.811055608065186728 ) ) ;
#740 = EDGE_LOOP ( 'NONE', ( #2992, #17252, #2513 ) ) ;
#741 = EDGE_CURVE ( 'NONE', #12240, #12970, #15109, .T. ) ;
#742 = CARTESIAN_POINT ( 'NONE',  ( -27.98221281347037959, 18.00000000000000355, 0.000000000000000000 ) ) ;
#743 = AXIS2_PLACEMENT_3D ( 'NONE', #8605, #17020, #646 ) ;
#744 = CARTESIAN_POINT ( 'NONE',  ( -75.75631164580342158, 193.9611582889532428, 24.29263104154016872 ) ) ;
#745 = PLANE ( 'NONE',  #2292 ) ;
#746 = DIRECTION ( 'NONE',  ( 0.000000000000000000, 0.000000000000000000, 1.000000000000000000 ) ) ;
#747 = AXIS2_PLACEMENT_3D ( 'NONE', #1269, #14466, #10656 ) ;
#748 = CARTESIAN_POINT ( 'NONE',  ( -95.00000000000000000, 171.6227766016838245, 0.000000000000000000 ) ) ;
#749 = ORIENTED_EDGE ( 'NONE', *, *, #15171, .F. ) ;
#750 = CYLINDRICAL_SURFACE ( 'NONE', #2202, 7.500000000000007105 ) ;
#751 = DIRECTION ( 'NONE',  ( -1.000000000000000000, 0.000000000000000000, 0.000000000000000000 ) ) ;
#752 = EDGE_LOOP ( 'NONE', ( #6021, #16237, #7652, #6565 ) ) ;
#753 = CARTESIAN_POINT ( 'NONE',  ( -44.99999999999997868, -20.00000000000000000, 40.00000000000000711 ) ) ;
#754 = PLANE ( 'NONE',  #14591 ) ;
#755 = ORIENTED_EDGE ( 'NONE', *, *, #1160, .T. ) ;
#756 = ORIENTED_EDGE ( 'NONE', *, *, #9201, .F. ) ;
#757 = ORIENTED_EDGE ( 'NONE', *, *, #700, .T. ) ;
#758 = AXIS2_PLACEMENT_3D ( 'NONE', #15657, #11594, #14252 ) ;
#759 = AXIS2_PLACEMENT_3D ( 'NONE', #15935, #15665, #6285 ) ;
#760 = AXIS2_PLACEMENT_3D ( 'NONE', #526, #3591, #2173 ) ;
#761 = ORIENTED_EDGE ( 'NONE', *, *, #2314, .F. ) ;
#762 = ADVANCED_FACE ( 'NONE', ( #2735, #8126 ), #14943, .F. ) ;
#763 = DIRECTION ( 'NONE',  ( -1.000000000000000000, -0.000000000000000000, -0.000000000000000000 ) ) ;
#764 = ORIENTED_EDGE ( 'NONE', *, *, #8937, .T. ) ;
#765 = SHAPE_REPRESENTATION_RELATIONSHIP ( 'NONE' , 'NONE' ,  #5345, #9102 ) ;
#766 = CARTESIAN_POINT ( 'NONE',  ( -207.6513770290094669, 172.0602489905835739, -0.7577244044828647107 ) ) ;
#767 = CARTESIAN_POINT ( 'NONE',  ( 6.471945315774715546, 134.1315750335306518, 12.99999999999999822 ) ) ;
#768 = DIRECTION ( 'NONE',  ( 1.000000000000000000, 0.000000000000000000, 0.000000000000000000 ) ) ;
#769 = CYLINDRICAL_SURFACE ( 'NONE', #12299, 20.00000000000000355 ) ;
#770 = EDGE_LOOP ( 'NONE', ( #2866, #6515, #15048, #9121 ) ) ;
#771 = FACE_BOUND ( 'NONE', #1719, .T. ) ;
#772 = DIRECTION ( 'NONE',  ( -0.000000000000000000, -0.000000000000000000, 1.000000000000000000 ) ) ;
#773 = AXIS2_PLACEMENT_3D ( 'NONE', #13462, #4256, #5749 ) ;
#774 = CARTESIAN_POINT ( 'NONE',  ( -153.0000000000000284, 171.6227766016838245, 11.93698985866628526 ) ) ;
#775 = AXIS2_PLACEMENT_3D ( 'NONE', #9067, #2340, #11897 ) ;
#776 = CARTESIAN_POINT ( 'NONE',  ( -14.56452549316047040, 20.00000000000115818, -9.027778560947799846 ) ) ;
#777 =( LENGTH_UNIT ( ) NAMED_UNIT ( * ) SI_UNIT ( .MILLI., .METRE. ) );
#778 = AXIS2_PLACEMENT_3D ( 'NONE', #2025, #16643, #10064 ) ;
#779 = ADVANCED_FACE ( 'NONE', ( #2020 ), #5919, .F. ) ;
#780 = CARTESIAN_POINT ( 'NONE',  ( 196.0000000000000000, 159.6227766016838814, -5.571800142134975431 ) ) ;
#781 = ORIENTED_EDGE ( 'NONE', *, *, #1682, .T. ) ;
#782 = ADVANCED_FACE ( 'NONE', ( #2094 ), #7493, .T. ) ;
#783 = FACE_OUTER_BOUND ( 'NONE', #7773, .T. ) ;
#784 = ORIENTED_EDGE ( 'NONE', *, *, #496, .T. ) ;
#785 = AXIS2_PLACEMENT_3D ( 'NONE', #9707, #16108, #10859 ) ;
#786 = CARTESIAN_POINT ( 'NONE',  ( 12.82244027866276426, 141.9777490571136696, 18.60671400555900235 ) ) ;
#787 = VECTOR ( 'NONE', #3451, 1000.000000000000000 ) ;
#788 = CIRCLE ( 'NONE', #8131, 5.000000000000000888 ) ;
#789 = DIRECTION ( 'NONE',  ( 0.9961946980917461003, 0.08715574274765185148, 0.000000000000000000 ) ) ;
#790 = EDGE_CURVE ( 'NONE', #4054, #1871, #14156, .T. ) ;
#791 = DIRECTION ( 'NONE',  ( -1.000000000000000000, 0.000000000000000000, 0.000000000000000000 ) ) ;
#792 = ADVANCED_FACE ( 'NONE', ( #11571 ), #7415, .T. ) ;
#793 = VERTEX_POINT ( 'NONE', #4418 ) ;
#794 = CARTESIAN_POINT ( 'NONE',  ( 34.93420767853316988, 19.99999999999999645, 0.000000000000000000 ) ) ;
#795 = CARTESIAN_POINT ( 'NONE',  ( 24.93507336697352628, 29.86842105263157876, -4.999999999999999112 ) ) ;
#796 = PLANE ( 'NONE',  #12731 ) ;
#797 = ORIENTED_EDGE ( 'NONE', *, *, #4142, .T. ) ;
#798 =( BOUNDED_CURVE ( )  B_SPLINE_CURVE ( 3, ( #13819, #11137, #7085, #11329 ),
 .UNSPECIFIED., .F., .F. ) 
 B_SPLINE_CURVE_WITH_KNOTS ( ( 4, 4 ),
 ( -8.881784197001252323E-16, 1.570796326794898556 ),
 .UNSPECIFIED. ) 
 CURVE ( )  GEOMETRIC_REPRESENTATION_ITEM ( )  RATIONAL_B_SPLINE_CURVE ( ( 1.000000000000000000, 0.8047378541243643824, 0.8047378541243643824, 1.000000000000000000 ) ) 
 REPRESENTATION_ITEM ( '' )  );
#799 = AXIS2_PLACEMENT_3D ( 'NONE', #5793, #6057, #1903 ) ;
#800 = ORIENTED_EDGE ( 'NONE', *, *, #1703, .F. ) ;
#801 = CARTESIAN_POINT ( 'NONE',  ( 17.68052782483612617, 29.96314637258912583, -14.61659083303745632 ) ) ;
#802 = AXIS2_PLACEMENT_3D ( 'NONE', #9199, #2579, #1331 ) ;
#803 =( GEOMETRIC_REPRESENTATION_CONTEXT ( 3 ) GLOBAL_UNCERTAINTY_ASSIGNED_CONTEXT ( ( #9704 ) ) GLOBAL_UNIT_ASSIGNED_CONTEXT ( ( #12385, #1419, #6983 ) ) REPRESENTATION_CONTEXT ( 'NONE', 'WORKASPACE' ) );
#804 = CARTESIAN_POINT ( 'NONE',  ( 25.63134405897505985, 139.9845197017440057, -9.403501633128708903 ) ) ;
#805 = VERTEX_POINT ( 'NONE', #8484 ) ;
#806 = CARTESIAN_POINT ( 'NONE',  ( -80.00000000000002842, 146.6227766016838245, 35.00200000000000244 ) ) ;
#807 = CARTESIAN_POINT ( 'NONE',  ( 6.714477151836450552, 134.0780154003031726, -13.00000000000000000 ) ) ;
#808 = ORIENTED_EDGE ( 'NONE', *, *, #995, .F. ) ;
#809 = DIRECTION ( 'NONE',  ( 0.000000000000000000, 0.000000000000000000, 1.000000000000000000 ) ) ;
#810 = VECTOR ( 'NONE', #1968, 1000.000000000000000 ) ;
#811 = AXIS2_PLACEMENT_3D ( 'NONE', #14678, #15827, #11740 ) ;
#812 = LINE ( 'NONE', #2307, #4993 ) ;
#813 = CARTESIAN_POINT ( 'NONE',  ( -95.00000000000000000, 171.6227766016838245, 0.000000000000000000 ) ) ;
#814 = CARTESIAN_POINT ( 'NONE',  ( -10.13698291596435119, 17.99999999999999645, 11.46558158188963539 ) ) ;
#815 = LINE ( 'NONE', #15940, #707 ) ;
#816 = CARTESIAN_POINT ( 'NONE',  ( 25.49999999999998579, 9.999999999999998224, 10.00000000000000178 ) ) ;
#817 = VERTEX_POINT ( 'NONE', #15375 ) ;
#819 = ORIENTED_EDGE ( 'NONE', *, *, #81, .F. ) ;
#818 = VECTOR ( 'NONE', #1736, 1000.000000000000000 ) ;
#820 = FACE_OUTER_BOUND ( 'NONE', #4191, .T. ) ;
#821 = VECTOR ( 'NONE', #4007, 1000.000000000000000 ) ;
#822 = FACE_OUTER_BOUND ( 'NONE', #15885, .T. ) ;
#823 = EDGE_CURVE ( 'NONE', #16300, #1130, #11027, .T. ) ;
#824 = CIRCLE ( 'NONE', #2229, 3.999999999999985789 ) ;
#825 = ORIENTED_EDGE ( 'NONE', *, *, #845, .T. ) ;
#826 = DIRECTION ( 'NONE',  ( -1.000000000000000000, 0.000000000000000000, 0.000000000000000000 ) ) ;
#827 = VECTOR ( 'NONE', #14654, 1000.000000000000000 ) ;
#828 = CARTESIAN_POINT ( 'NONE',  ( 19.05951714192248403, 29.94485528828719367, 14.11495713418740294 ) ) ;
#829 = ORIENTED_EDGE ( 'NONE', *, *, #7545, .T. ) ;
#830 = CARTESIAN_POINT ( 'NONE',  ( 196.0000000000000000, 187.6227766016837961, 12.50000337241049309 ) ) ;
#831 = DIRECTION ( 'NONE',  ( -1.000000000000000000, 0.000000000000000000, 0.000000000000000000 ) ) ;
#832 = VECTOR ( 'NONE', #2538, 1000.000000000000000 ) ;
#833 = CARTESIAN_POINT ( 'NONE',  ( -15.84744341939753021, 31.82541372190370055, -11.32583567006417624 ) ) ;
#834 = AXIS2_PLACEMENT_3D ( 'NONE', #9039, #6477, #17278 ) ;
#835 = CARTESIAN_POINT ( 'NONE',  ( 49.99999999999998579, 167.6227766016838814, -19.42820660268601074 ) ) ;
#836 = CIRCLE ( 'NONE', #4239, 5.000000000000007994 ) ;
#837 = ORIENTED_EDGE ( 'NONE', *, *, #15585, .T. ) ;
#838 = CYLINDRICAL_SURFACE ( 'NONE', #7299, 5.000000000000000888 ) ;
#839 = CARTESIAN_POINT ( 'NONE',  ( -26.10410744458348020, 20.00000000000000000, -13.37721135299797659 ) ) ;
#840 = ORIENTED_EDGE ( 'NONE', *, *, #4013, .T. ) ;
#841 = CARTESIAN_POINT ( 'NONE',  ( -207.2467692809710229, 174.8522807748693708, -4.001497440111938531 ) ) ;
#842 = CARTESIAN_POINT ( 'NONE',  ( -40.00000000000000000, 4.000000000000000000, -33.00000000000000711 ) ) ;
#843 = EDGE_CURVE ( 'NONE', #7078, #17487, #4766, .T. ) ;
#844 = ORIENTED_EDGE ( 'NONE', *, *, #10151, .T. ) ;
#845 = EDGE_CURVE ( 'NONE', #12168, #14104, #5943, .T. ) ;
#846 = VERTEX_POINT ( 'NONE', #7154 ) ;
#847 = EDGE_CURVE ( 'NONE', #16728, #15915, #15300, .T. ) ;
#848 = ORIENTED_EDGE ( 'NONE', *, *, #17042, .F. ) ;
#849 = EDGE_CURVE ( 'NONE', #13616, #7959, #8196, .T. ) ;
#850 = AXIS2_PLACEMENT_3D ( 'NONE', #4169, #5324, #16475 ) ;
#851 = DIRECTION ( 'NONE',  ( 0.000000000000000000, -2.891205793294676354E-16, -1.000000000000000000 ) ) ;
#852 = VECTOR ( 'NONE', #2578, 1000.000000000000000 ) ;
#853 = EDGE_LOOP ( 'NONE', ( #13360, #10360 ) ) ;
#854 = DIRECTION ( 'NONE',  ( 0.000000000000000000, 0.000000000000000000, 1.000000000000000000 ) ) ;
#855 = CARTESIAN_POINT ( 'NONE',  ( -13.87134331504352325, 32.05147385205248867, 10.53504704850738705 ) ) ;
#856 = SURFACE_STYLE_FILL_AREA ( #11204 ) ;
#857 = DIRECTION ( 'NONE',  ( 0.000000000000000000, 0.000000000000000000, -1.000000000000000000 ) ) ;
#858 = DIRECTION ( 'NONE',  ( 0.000000000000000000, 0.000000000000000000, 1.000000000000000000 ) ) ;
#859 = DIRECTION ( 'NONE',  ( -0.08715574274764689711, 0.9961946980917465444, 0.000000000000000000 ) ) ;
#860 = EDGE_LOOP ( 'NONE', ( #844, #11416 ) ) ;
#861 = CARTESIAN_POINT ( 'NONE',  ( 26.51307711398865408, 139.5431919169737967, 7.747420853565629706 ) ) ;
#862 = VECTOR ( 'NONE', #2805, 1000.000000000000000 ) ;
#863 = DIRECTION ( 'NONE',  ( 0.000000000000000000, 0.000000000000000000, -1.000000000000000000 ) ) ;
#864 = CARTESIAN_POINT ( 'NONE',  ( 39.99999999999998579, 4.000000000000000000, -33.00000000000000000 ) ) ;
#865 = ADVANCED_FACE ( 'NONE', ( #12551, #9893 ), #417, .F. ) ;
#866 = AXIS2_PLACEMENT_3D ( 'NONE', #16436, #16167, #6863 ) ;
#867 = CARTESIAN_POINT ( 'NONE',  ( -15.30535435590778448, 19.99999999999766587, -5.925683940270866756 ) ) ;
#868 = DIRECTION ( 'NONE',  ( -1.000000000000000000, 0.000000000000000000, 0.000000000000000000 ) ) ;
#869 = CARTESIAN_POINT ( 'NONE',  ( 25.52968048427065284, 198.8808217108463055, 18.60648811928370350 ) ) ;
#870 = ORIENTED_EDGE ( 'NONE', *, *, #16889, .F. ) ;
#871 = CARTESIAN_POINT ( 'NONE',  ( 0.000000000000000000, 20.00000000000000000, 0.000000000000000000 ) ) ;
#872 = CARTESIAN_POINT ( 'NONE',  ( 48.00000000000000711, 175.6227766016838245, 5.571800142134975431 ) ) ;
#873 = CIRCLE ( 'NONE', #2278, 5.000000000000004441 ) ;
#874 = VERTEX_POINT ( 'NONE', #7331 ) ;
#875 = DIRECTION ( 'NONE',  ( 0.000000000000000000, 0.9938079899999064937, -0.1111111111111109523 ) ) ;
#876 = AXIS2_PLACEMENT_3D ( 'NONE', #4470, #9943, #1984 ) ;
#877 = CARTESIAN_POINT ( 'NONE',  ( -192.9999999999999716, 171.6227766016838245, 14.16444493696511486 ) ) ;
#878 = DIRECTION ( 'NONE',  ( 1.000000000000000000, 0.000000000000000000, 0.000000000000000000 ) ) ;
#879 = ORIENTED_EDGE ( 'NONE', *, *, #15983, .F. ) ;
#880 = CARTESIAN_POINT ( 'NONE',  ( -45.00000000000000711, -20.00000000000000000, -40.00000000000000000 ) ) ;
#881 = DIRECTION ( 'NONE',  ( 0.000000000000000000, 1.000000000000000000, 0.000000000000000000 ) ) ;
#882 = ADVANCED_FACE ( 'NONE', ( #12736 ), #11219, .T. ) ;
#883 = DIRECTION ( 'NONE',  ( -0.000000000000000000, -0.000000000000000000, -1.000000000000000000 ) ) ;
#884 = EDGE_CURVE ( 'NONE', #11970, #4566, #15562, .T. ) ;
#885 = CARTESIAN_POINT ( 'NONE',  ( 24.16572647217576275, 198.0686797691926131, -22.93241811017415088 ) ) ;
#886 = ORIENTED_EDGE ( 'NONE', *, *, #9910, .T. ) ;
#887 = CIRCLE ( 'NONE', #13615, 8.000000000000000000 ) ;
#888 = ORIENTED_EDGE ( 'NONE', *, *, #11863, .T. ) ;
#889 = CARTESIAN_POINT ( 'NONE',  ( 22.52789404479186786, 19.99999999999999289, -11.66574595783169954 ) ) ;
#890 = CARTESIAN_POINT ( 'NONE',  ( 10.67016715011969374, 138.9541284244158419, -13.78020913810582115 ) ) ;
#891 = ORIENTED_EDGE ( 'NONE', *, *, #2427, .F. ) ;
#892 = FACE_OUTER_BOUND ( 'NONE', #9411, .T. ) ;
#893 = ADVANCED_FACE ( 'NONE', ( #4594 ), #514, .F. ) ;
#894 = CARTESIAN_POINT ( 'NONE',  ( 27.50000000000001066, 146.6227766016838245, -16.00000000000000000 ) ) ;
#895 = ORIENTED_EDGE ( 'NONE', *, *, #16793, .T. ) ;
#896 = DIRECTION ( 'NONE',  ( 1.000000000000000000, 0.000000000000000000, -0.000000000000000000 ) ) ;
#897 = DIRECTION ( 'NONE',  ( 1.000000000000000000, 0.000000000000000000, -0.000000000000000000 ) ) ;
#898 =( BOUNDED_SURFACE ( )  B_SPLINE_SURFACE ( 3, 2, ( 
 ( #1065, #3809, #6207 ),
 ( #2308, #11859, #5143 ),
 ( #9204, #14610, #2482 ),
 ( #7880, #13289, #14785 ),
 ( #2750, #13372, #9295 ),
 ( #6736, #8475, #13891 ),
 ( #1750, #7145, #13552 ),
 ( #12137, #6646, #3074 ),
 ( #15197, #4004, #16129 ),
 ( #10716, #16028, #12041 ),
 ( #7968, #4078, #6826 ),
 ( #8051, #12218, #12544 ),
 ( #5488, #10619, #410 ),
 ( #16212, #1335, #9384 ),
 ( #2659, #5320, #13461 ),
 ( #1426, #9459, #7 ),
 ( #5411, #10802, #5816 ),
 ( #14869, #8140, #89 ),
 ( #11207, #5223, #10875 ),
 ( #3908, #16294, #14705 ),
 ( #4166, #9550, #2583 ),
 ( #1239, #17446, #16102 ),
 ( #3614, #7675, #2458 ),
 ( #9003, #13170, #1132 ),
 ( #5291, #3977, #11924 ),
 ( #7756, #13084, #1216 ),
 ( #14496, #10690, #9361 ),
 ( #13262, #7947, #2364 ) ),
 .UNSPECIFIED., .F., .F., .F. ) 
 B_SPLINE_SURFACE_WITH_KNOTS ( ( 4, 2, 2, 2, 2, 2, 2, 2, 2, 2, 2, 2, 2, 4 ),
 ( 3, 3 ),
 ( 0.01342997177288655399, 0.01733910390705692070, 0.01929366997414210666, 0.02124823604122728915, 0.02515736817539765760, 0.02711193424248284356, 0.02906650030956802605, 0.03297563244373839797, 0.03493019851082358046, 0.03688476457790876295, 0.03883933064499394544, 0.03981661367853653322, 0.04079389671207912793, 0.04470302884624949985 ),
 ( 0.000000000000000000, 1.000000000000000000 ),
 .UNSPECIFIED. ) 
 GEOMETRIC_REPRESENTATION_ITEM ( )  RATIONAL_B_SPLINE_SURFACE ( (
 ( 1.000000000000000000, 0.7117435966472906994, 1.000000000000000000),
 ( 1.000000000000000000, 0.7117434842622243352, 1.000000000000000000),
 ( 1.000000000000000000, 0.7117144184577041122, 1.000000000000000000),
 ( 1.000000000000000000, 0.7116285301813174424, 1.000000000000000000),
 ( 1.000000000000000000, 0.7115928256594988843, 1.000000000000000000),
 ( 1.000000000000000000, 0.7115068832447583036, 1.000000000000000000),
 ( 1.000000000000000000, 0.7114564033772057261, 1.000000000000000000),
 ( 1.000000000000000000, 0.7112861117249480447, 1.000000000000000000),
 ( 1.000000000000000000, 0.7111469280185451769, 1.000000000000000000),
 ( 1.000000000000000000, 0.7108993804763810154, 1.000000000000000000),
 ( 1.000000000000000000, 0.7108100171490865371, 1.000000000000000000),
 ( 1.000000000000000000, 0.7106191415567553182, 1.000000000000000000),
 ( 1.000000000000000000, 0.7105185320923615988, 1.000000000000000000),
 ( 1.000000000000000000, 0.7102014790723295556, 1.000000000000000000),
 ( 1.000000000000000000, 0.7099699576740480245, 1.000000000000000000),
 ( 1.000000000000000000, 0.7095909300315041968, 1.000000000000000000),
 ( 1.000000000000000000, 0.7094593121158984106, 1.000000000000000000),
 ( 1.000000000000000000, 0.7091910831477740151, 1.000000000000000000),
 ( 1.000000000000000000, 0.7090537746377550965, 1.000000000000000000),
 ( 1.000000000000000000, 0.7087727591781153302, 1.000000000000000000),
 ( 1.000000000000000000, 0.7086290523620303317, 1.000000000000000000),
 ( 1.000000000000000000, 0.7084085592173990920, 1.000000000000000000),
 ( 1.000000000000000000, 0.7083342380281847372, 1.000000000000000000),
 ( 1.000000000000000000, 0.7081839094109132482, 1.000000000000000000),
 ( 1.000000000000000000, 0.7081077478408333015, 1.000000000000000000),
 ( 1.000000000000000000, 0.7077267031860466906, 1.000000000000000000),
 ( 1.000000000000000000, 0.7074184602291956336, 1.000000000000000000),
 ( 1.000000000000000000, 0.7071067811865476838, 1.000000000000000000) ) ) 
 REPRESENTATION_ITEM ( '' )  SURFACE ( )  );
#899 = DIRECTION ( 'NONE',  ( -0.000000000000000000, -1.000000000000000000, -0.000000000000000000 ) ) ;
#900 = CARTESIAN_POINT ( 'NONE',  ( -13.23954943057894873, 31.86042443463173157, 11.05847410484002680 ) ) ;
#901 = CARTESIAN_POINT ( 'NONE',  ( -27.99999999999998224, 10.00000000000000000, 0.000000000000000000 ) ) ;
#902 = CARTESIAN_POINT ( 'NONE',  ( 28.95071320099337697, 140.7094120356993585, -16.41247553121493041 ) ) ;
#903 = VERTEX_POINT ( 'NONE', #3255 ) ;
#904 = FACE_OUTER_BOUND ( 'NONE', #13730, .T. ) ;
#905 = ORIENTED_EDGE ( 'NONE', *, *, #16605, .T. ) ;
#906 = CARTESIAN_POINT ( 'NONE',  ( 49.99999999999998579, 171.6227766016838245, 12.50000337241049131 ) ) ;
#907 = CARTESIAN_POINT ( 'NONE',  ( -32.66708739526796279, 119.0000000000000284, 4.722170599040653727 ) ) ;
#908 = ORIENTED_EDGE ( 'NONE', *, *, #8104, .T. ) ;
#909 = CARTESIAN_POINT ( 'NONE',  ( -80.00000000000001421, 196.6227766016838245, -12.99999999999999822 ) ) ;
#910 = ADVANCED_FACE ( 'NONE', ( #609 ), #8658, .F. ) ;
#911 = FACE_OUTER_BOUND ( 'NONE', #5499, .T. ) ;
#912 = CARTESIAN_POINT ( 'NONE',  ( 23.61360151038711308, 29.88540148010350705, 10.01045486545366181 ) ) ;
#913 = ORIENTED_EDGE ( 'NONE', *, *, #1538, .F. ) ;
#914 = CARTESIAN_POINT ( 'NONE',  ( 48.00000000000000711, 175.6227766016838530, -19.42820660268601074 ) ) ;
#915 = CARTESIAN_POINT ( 'NONE',  ( 2.950000000000001066, 0.000000000000000000, 2.499999999999999112 ) ) ;
#916 = DIRECTION ( 'NONE',  ( 0.000000000000000000, 0.000000000000000000, 1.000000000000000000 ) ) ;
#917 = EDGE_CURVE ( 'NONE', #1967, #544, #4724, .T. ) ;
#918 = CARTESIAN_POINT ( 'NONE',  ( -9.672962866393921999, 30.74839102026217574, -12.74052981562734388 ) ) ;
#919 = VERTEX_POINT ( 'NONE', #8995 ) ;
#920 = CARTESIAN_POINT ( 'NONE',  ( 48.00000000000000711, 155.6227766016839098, 15.00000337241049486 ) ) ;
#921 = ORIENTED_EDGE ( 'NONE', *, *, #5460, .T. ) ;
#922 = CARTESIAN_POINT ( 'NONE',  ( 36.00000000000000711, 196.6227766016838245, -24.49489742783179125 ) ) ;
#923 = DIRECTION ( 'NONE',  ( 0.000000000000000000, 1.387778780781445676E-14, -1.000000000000000000 ) ) ;
#924 = ORIENTED_EDGE ( 'NONE', *, *, #4888, .T. ) ;
#925 = VERTEX_POINT ( 'NONE', #11652 ) ;
#926 = ORIENTED_EDGE ( 'NONE', *, *, #9179, .F. ) ;
#927 = CARTESIAN_POINT ( 'NONE',  ( -86.08967107480829384, 151.0287754819113957, -25.78994361341036168 ) ) ;
#928 = ORIENTED_EDGE ( 'NONE', *, *, #4621, .F. ) ;
#929 = DIRECTION ( 'NONE',  ( 0.000000000000000000, 0.000000000000000000, 1.000000000000000000 ) ) ;
#930 = CARTESIAN_POINT ( 'NONE',  ( 15.60228996708985072, 124.9392590763940518, -1.450155947765682260E-14 ) ) ;
#931 = LINE ( 'NONE', #1013, #7504 ) ;
#932 = CARTESIAN_POINT ( 'NONE',  ( 25.68041636605677525, 150.8057096996395217, -28.13880055569950400 ) ) ;
#933 = ADVANCED_FACE ( 'NONE', ( #1126 ), #13158, .F. ) ;
#934 = CARTESIAN_POINT ( 'NONE',  ( 23.09107716886297013, 17.99999999999083045, 5.538990817933215460 ) ) ;
#935 = EDGE_CURVE ( 'NONE', #15663, #15092, #15839, .T. ) ;
#936 = CARTESIAN_POINT ( 'NONE',  ( -50.00000000000000000, 191.6227766016837961, 1.224646799147353454E-15 ) ) ;
#937 = EDGE_CURVE ( 'NONE', #1279, #14899, #10582, .T. ) ;
#938 = VERTEX_POINT ( 'NONE', #7842 ) ;
#939 = CARTESIAN_POINT ( 'NONE',  ( 48.00000000000000711, 179.6227766016838245, -12.50000337241049309 ) ) ;
#940 = CARTESIAN_POINT ( 'NONE',  ( 20.22393135579957502, 29.92951751662230109, -13.49252536210626197 ) ) ;
#941 = DIRECTION ( 'NONE',  ( -0.000000000000000000, -0.000000000000000000, -1.000000000000000000 ) ) ;
#942 = CARTESIAN_POINT ( 'NONE',  ( 17.53512989260226362, 29.96507997281579350, 14.66107963853301399 ) ) ;
#943 = ORIENTED_EDGE ( 'NONE', *, *, #15549, .T. ) ;
#944 = FACE_OUTER_BOUND ( 'NONE', #7191, .T. ) ;
#945 = CARTESIAN_POINT ( 'NONE',  ( 30.21607733469937429, 201.6195082837481038, 13.75486997215867291 ) ) ;
#946 = ORIENTED_EDGE ( 'NONE', *, *, #5353, .F. ) ;
#947 = DIRECTION ( 'NONE',  ( 0.000000000000000000, 0.000000000000000000, -1.000000000000000000 ) ) ;
#948 = ORIENTED_EDGE ( 'NONE', *, *, #5128, .T. ) ;
#949 = CARTESIAN_POINT ( 'NONE',  ( -79.08361844431172472, 141.7021811473759669, 13.91989935049637062 ) ) ;
#950 = DIRECTION ( 'NONE',  ( 1.000000000000000000, 0.000000000000000000, 0.000000000000000000 ) ) ;
#951 = CARTESIAN_POINT ( 'NONE',  ( 49.99999999999998579, 183.6227766016837961, -5.571800142134975431 ) ) ;
#952 = CARTESIAN_POINT ( 'NONE',  ( 7.438682885632053932, 133.7774783946093464, -12.91151668396746111 ) ) ;
#953 = ORIENTED_EDGE ( 'NONE', *, *, #16168, .T. ) ;
#954 = LINE ( 'NONE', #17334, #5584 ) ;
#955 = CARTESIAN_POINT ( 'NONE',  ( 0.000000000000000000, 2.000000000000000000, 0.000000000000000000 ) ) ;
#956 = CARTESIAN_POINT ( 'NONE',  ( 48.00000000000000000, 196.6227766016838245, 0.000000000000000000 ) ) ;
#957 = CARTESIAN_POINT ( 'NONE',  ( 30.55142212064656704, 202.6030615872001590, -16.28580987144873404 ) ) ;
#958 = ORIENTED_EDGE ( 'NONE', *, *, #11073, .T. ) ;
#959 = ORIENTED_EDGE ( 'NONE', *, *, #13344, .T. ) ;
#960 = CARTESIAN_POINT ( 'NONE',  ( 14.93242934743711814, 20.00000000000000000, -24.99999999999999645 ) ) ;
#961 = VECTOR ( 'NONE', #878, 1000.000000000000000 ) ;
#962 = CARTESIAN_POINT ( 'NONE',  ( 8.038468667238035437, 139.4170824625289242, -14.76281475457819070 ) ) ;
#963 = ORIENTED_EDGE ( 'NONE', *, *, #823, .F. ) ;
#964 = CARTESIAN_POINT ( 'NONE',  ( -76.65341708795939724, 151.6073998100962399, -28.71242994986354446 ) ) ;
#965 = CARTESIAN_POINT ( 'NONE',  ( 10.58901158398830766, 139.9616134764785329, -11.54438095561596000 ) ) ;
#966 = ORIENTED_EDGE ( 'NONE', *, *, #5460, .F. ) ;
#967 = DIRECTION ( 'NONE',  ( -0.000000000000000000, -0.000000000000000000, -1.000000000000000000 ) ) ;
#968 = EDGE_CURVE ( 'NONE', #15581, #8813, #1708, .T. ) ;
#969 = DIRECTION ( 'NONE',  ( -1.000000000000000000, -0.000000000000000000, -0.000000000000000000 ) ) ;
#970 = FACE_OUTER_BOUND ( 'NONE', #1823, .T. ) ;
#971 = VECTOR ( 'NONE', #8694, 1000.000000000000000 ) ;
#972 = DIRECTION ( 'NONE',  ( -0.000000000000000000, 0.000000000000000000, -1.000000000000000000 ) ) ;
#973 = CARTESIAN_POINT ( 'NONE',  ( -12.54944958582184888, 31.64997543288135873, 11.54276402733058937 ) ) ;
#974 = DIRECTION ( 'NONE',  ( -0.000000000000000000, -0.000000000000000000, -1.000000000000000000 ) ) ;
#975 = CARTESIAN_POINT ( 'NONE',  ( 48.00000000000000711, 151.6227766016839098, -5.571800142134973655 ) ) ;
#976 = ORIENTED_EDGE ( 'NONE', *, *, #11728, .F. ) ;
#977 = DIRECTION ( 'NONE',  ( -0.000000000000000000, -0.000000000000000000, -1.000000000000000000 ) ) ;
#978 = VERTEX_POINT ( 'NONE', #10499 ) ;
#979 = CARTESIAN_POINT ( 'NONE',  ( -27.99999999999998224, 10.00000000000000000, -35.00200000000000244 ) ) ;
#980 = CARTESIAN_POINT ( 'NONE',  ( -45.00000000000001421, -20.00000000000000000, 35.00000000000000711 ) ) ;
#981 = ORIENTED_EDGE ( 'NONE', *, *, #16898, .T. ) ;
#982 = FACE_OUTER_BOUND ( 'NONE', #16917, .T. ) ;
#983 = CARTESIAN_POINT ( 'NONE',  ( 25.87766738269754541, 139.8661988410599406, 8.984976992518891592 ) ) ;
#984 = CIRCLE ( 'NONE', #416, 2.500000000000000000 ) ;
#985 = AXIS2_PLACEMENT_3D ( 'NONE', #17428, #10947, #13359 ) ;
#986 = CARTESIAN_POINT ( 'NONE',  ( 34.42312820345349422, 19.99999999999999645, 9.539278825327816236 ) ) ;
#987 = EDGE_CURVE ( 'NONE', #6662, #12168, #15905, .T. ) ;
#988 = ORIENTED_EDGE ( 'NONE', *, *, #13000, .T. ) ;
#989 = FACE_OUTER_BOUND ( 'NONE', #6924, .T. ) ;
#990 = CARTESIAN_POINT ( 'NONE',  ( -73.00000000000001421, 171.6227766016838245, 0.000000000000000000 ) ) ;
#991 = EDGE_CURVE ( 'NONE', #12595, #8470, #13689, .T. ) ;
#992 = DIRECTION ( 'NONE',  ( -1.000000000000000000, 0.000000000000000000, 0.000000000000000000 ) ) ;
#993 = CARTESIAN_POINT ( 'NONE',  ( -12.63609539511579527, 18.00000000000000000, -24.35132453916584794 ) ) ;
#994 = EDGE_CURVE ( 'NONE', #3454, #1173, #14, .T. ) ;
#995 = EDGE_CURVE ( 'NONE', #13884, #3234, #12362, .T. ) ;
#996 = ORIENTED_EDGE ( 'NONE', *, *, #2991, .F. ) ;
#997 = DIRECTION ( 'NONE',  ( 0.000000000000000000, 0.000000000000000000, 1.000000000000000000 ) ) ;
#998 = VECTOR ( 'NONE', #6430, 1000.000000000000000 ) ;
#999 = ORIENTED_EDGE ( 'NONE', *, *, #17387, .F. ) ;
#1000 = CARTESIAN_POINT ( 'NONE',  ( 24.96063036748655506, 193.3606217133605298, -27.43184792633611480 ) ) ;
#1001 = AXIS2_PLACEMENT_3D ( 'NONE', #7737, #14563, #8984 ) ;
#1002 = DIRECTION ( 'NONE',  ( -1.000000000000000000, 0.000000000000000000, 0.000000000000000000 ) ) ;
#1003 = ORIENTED_EDGE ( 'NONE', *, *, #9588, .F. ) ;
#1004 = ORIENTED_EDGE ( 'NONE', *, *, #6432, .T. ) ;
#1005 = EDGE_LOOP ( 'NONE', ( #12594, #1908, #10659, #13298, #353 ) ) ;
#1006 = CARTESIAN_POINT ( 'NONE',  ( -87.46328901163954583, 147.3890553372962700, -22.40111672564486867 ) ) ;
#1007 = UNCERTAINTY_MEASURE_WITH_UNIT (LENGTH_MEASURE( 1.000000000000000082E-05 ), #2734, 'distance_accuracy_value', 'NONE');
#1008 = AXIS2_PLACEMENT_3D ( 'NONE', #5879, #5974, #474 ) ;
#1009 = ORIENTED_EDGE ( 'NONE', *, *, #607, .T. ) ;
#1010 = DIRECTION ( 'NONE',  ( 1.000000000000000000, 0.000000000000000000, 0.000000000000000000 ) ) ;
#1011 = DIRECTION ( 'NONE',  ( -1.000000000000000000, 0.000000000000000000, 0.000000000000000000 ) ) ;
#1012 = AXIS2_PLACEMENT_3D ( 'NONE', #2075, #11376, #7558 ) ;
#1013 = CARTESIAN_POINT ( 'NONE',  ( 21.99999999999998224, 9.999999999999998224, -35.00000000000000000 ) ) ;
#1014 = CARTESIAN_POINT ( 'NONE',  ( 17.00000000000000000, 171.6227766016838245, 20.00000000000000355 ) ) ;
#1015 = CARTESIAN_POINT ( 'NONE',  ( 22.25017171248248005, 17.99999999999771916, 8.611421531743401303 ) ) ;
#1016 = DIRECTION ( 'NONE',  ( 1.000000000000000000, 0.000000000000000000, -0.000000000000000000 ) ) ;
#1017 = ORIENTED_EDGE ( 'NONE', *, *, #8652, .T. ) ;
#1018 = CARTESIAN_POINT ( 'NONE',  ( 27.44407568426044008, 138.8271129316868837, 3.666666666666658081 ) ) ;
#1019 = CARTESIAN_POINT ( 'NONE',  ( -25.49999999999998579, 10.00000000000000000, -16.00000000000000000 ) ) ;
#1020 = DIRECTION ( 'NONE',  ( -0.000000000000000000, -0.000000000000000000, -1.000000000000000000 ) ) ;
#1021 = DIRECTION ( 'NONE',  ( 0.000000000000000000, 0.000000000000000000, -1.000000000000000000 ) ) ;
#1022 = DIRECTION ( 'NONE',  ( 0.000000000000000000, -1.000000000000000000, -6.123233995736762338E-17 ) ) ;
#1023 = ORIENTED_EDGE ( 'NONE', *, *, #8940, .T. ) ;
#1024 = DIRECTION ( 'NONE',  ( 0.000000000000000000, 0.000000000000000000, -1.000000000000000000 ) ) ;
#1025 = AXIS2_PLACEMENT_3D ( 'NONE', #98, #12307, #8152 ) ;
#1026 = TOROIDAL_SURFACE ( 'NONE', #8943, -78.75916623668499028, 108.0000000000000142 ) ;
#1027 = AXIS2_PLACEMENT_3D ( 'NONE', #6143, #14706, #8870 ) ;
#1028 = CIRCLE ( 'NONE', #3301, 2.000000000000001776 ) ;
#1029 = DIRECTION ( 'NONE',  ( 1.000000000000000000, 0.000000000000000000, 0.000000000000000000 ) ) ;
#1030 = EDGE_CURVE ( 'NONE', #160, #8896, #6960, .T. ) ;
#1031 = EDGE_CURVE ( 'NONE', #9988, #1445, #13577, .T. ) ;
#1032 = ADVANCED_FACE ( 'NONE', ( #10848 ), #9355, .F. ) ;
#1033 = EDGE_LOOP ( 'NONE', ( #17321, #14333 ) ) ;
#1034 =( NAMED_UNIT ( * ) SI_UNIT ( $, .STERADIAN. ) SOLID_ANGLE_UNIT ( ) );
#1035 = FACE_OUTER_BOUND ( 'NONE', #10686, .T. ) ;
#1036 = VERTEX_POINT ( 'NONE', #6706 ) ;
#1037 =( LENGTH_UNIT ( ) NAMED_UNIT ( * ) SI_UNIT ( .MILLI., .METRE. ) );
#1038 = CARTESIAN_POINT ( 'NONE',  ( -82.95659350918997177, 142.5787592618052315, 15.67196037041395229 ) ) ;
#1040 = DIRECTION ( 'NONE',  ( 1.000000000000000000, 0.000000000000000000, 0.000000000000000000 ) ) ;
#1039 = AXIS2_PLACEMENT_3D ( 'NONE', #16734, #11404, #12560 ) ;
#1041 = CARTESIAN_POINT ( 'NONE',  ( -85.96511341109068383, 145.8838445361196818, -23.72313757307397708 ) ) ;
#1042 = CIRCLE ( 'NONE', #1617, 12.00000000000000000 ) ;
#1043 = CARTESIAN_POINT ( 'NONE',  ( 12.04170873690402566, 130.2202688438208327, -11.06482237631273868 ) ) ;
#1044 = VERTEX_POINT ( 'NONE', #16092 ) ;
#1045 = DIRECTION ( 'NONE',  ( -0.000000000000000000, -0.000000000000000000, 1.000000000000000000 ) ) ;
#1046 = CARTESIAN_POINT ( 'NONE',  ( -96.00000000000001421, 171.6227766016838245, 0.000000000000000000 ) ) ;
#1047 = CARTESIAN_POINT ( 'NONE',  ( 196.0000000000000000, 179.6227766016838245, -10.00000337241049309 ) ) ;
#1048 = B_SPLINE_CURVE_WITH_KNOTS ( 'NONE', 3,
 ( #12094, #12187, #1202, #6519, #10675, #4125, #1292, #10927, #56, #16350, #4049, #11910, #9347, #7932, #5456, #17316, #14830, #4218, #5184, #6605, #17502, #15985 ),
 .UNSPECIFIED., .F., .F.,
 ( 4, 2, 2, 2, 2, 2, 2, 2, 2, 2, 4 ),
 ( 0.000000000000000000, 0.002375333402909271790, 0.004750666805818540978, 0.007126000208727810599, 0.009501333611637081955, 0.01068900031309169378, 0.01187666701454630908, 0.01425200041745553273, 0.01543966711891012200, 0.01662733382036471128, 0.01900266722327392452 ),
 .UNSPECIFIED. ) ;
#1049 = ORIENTED_EDGE ( 'NONE', *, *, #6936, .F. ) ;
#1050 = ORIENTED_EDGE ( 'NONE', *, *, #14204, .T. ) ;
#1051 = DIRECTION ( 'NONE',  ( -1.000000000000000000, -0.000000000000000000, -0.000000000000000000 ) ) ;
#1052 = EDGE_CURVE ( 'NONE', #16728, #16016, #10683, .T. ) ;
#1053 = ADVANCED_FACE ( 'NONE', ( #4053 ), #5637, .F. ) ;
#1054 = AXIS2_PLACEMENT_3D ( 'NONE', #7576, #6422, #2176 ) ;
#1055 = VERTEX_POINT ( 'NONE', #13520 ) ;
#1056 = DIRECTION ( 'NONE',  ( 0.000000000000000000, -1.000000000000000000, 7.341990890863118602E-16 ) ) ;
#1057 = EDGE_CURVE ( 'NONE', #5440, #4930, #14430, .T. ) ;
#1058 = CARTESIAN_POINT ( 'NONE',  ( 12.23870813552851722, 139.5070109101417302, -10.31054875319186515 ) ) ;
#1059 = ORIENTED_EDGE ( 'NONE', *, *, #1533, .T. ) ;
#1060 = DIRECTION ( 'NONE',  ( 1.000000000000000000, 0.000000000000000000, 0.000000000000000000 ) ) ;
#1061 = CARTESIAN_POINT ( 'NONE',  ( -43.00000000000000000, 130.0000000000000000, 15.00000000000000000 ) ) ;
#1062 = CARTESIAN_POINT ( 'NONE',  ( 0.000000000000000000, 0.000000000000000000, 0.000000000000000000 ) ) ;
#1063 = CARTESIAN_POINT ( 'NONE',  ( -90.80384757729339640, 204.6227766016838245, 0.000000000000000000 ) ) ;
#1064 = DIRECTION ( 'NONE',  ( -0.000000000000000000, -0.000000000000000000, 1.000000000000000000 ) ) ;
#1065 = CARTESIAN_POINT ( 'NONE',  ( 22.93524650466160253, 29.84210526315789025, -5.000000000000003553 ) ) ;
#1066 = DIRECTION ( 'NONE',  ( -1.000000000000000000, 0.000000000000000000, 0.000000000000000000 ) ) ;
#1067 = CARTESIAN_POINT ( 'NONE',  ( -72.50000000000002842, 146.6227766016838245, -13.00000000000000000 ) ) ;
#1068 = AXIS2_PLACEMENT_3D ( 'NONE', #3841, #36, #5435 ) ;
#1069 = CARTESIAN_POINT ( 'NONE',  ( -725.0000000000000000, 19.99999999999995737, 13.00000000000000000 ) ) ;
#1070 = AXIS2_PLACEMENT_3D ( 'NONE', #12538, #13961, #9879 ) ;
#1071 = CARTESIAN_POINT ( 'NONE',  ( -45.00000000000003553, 120.0000000000000142, -4.999999999999999112 ) ) ;
#1072 = ORIENTED_EDGE ( 'NONE', *, *, #10985, .T. ) ;
#1073 = CYLINDRICAL_SURFACE ( 'NONE', #5904, 9.999999999999994671 ) ;
#1074 = VERTEX_POINT ( 'NONE', #5461 ) ;
#1075 = EDGE_CURVE ( 'NONE', #1461, #805, #9519, .T. ) ;
#1076 = DIRECTION ( 'NONE',  ( -1.000000000000000000, 0.000000000000000000, -8.673617379884037937E-17 ) ) ;
#1077 = DIRECTION ( 'NONE',  ( -0.000000000000000000, -0.000000000000000000, 1.000000000000000000 ) ) ;
#1078 = ORIENTED_EDGE ( 'NONE', *, *, #14042, .F. ) ;
#1079 = CARTESIAN_POINT ( 'NONE',  ( 48.00000000000000000, 171.6227766016838245, -15.00000337241049131 ) ) ;
#1080 = CARTESIAN_POINT ( 'NONE',  ( 26.57417986947462651, 139.5089559931849692, 7.600184560211070917 ) ) ;
#1081 = ORIENTED_EDGE ( 'NONE', *, *, #7693, .F. ) ;
#1082 = VECTOR ( 'NONE', #2070, 1000.000000000000000 ) ;
#1083 = CARTESIAN_POINT ( 'NONE',  ( -151.9615242270660929, 171.6227766016838245, 0.000000000000000000 ) ) ;
#1084 = VECTOR ( 'NONE', #3089, 1000.000000000000000 ) ;
#1085 = ORIENTED_EDGE ( 'NONE', *, *, #3481, .T. ) ;
#1086 = CARTESIAN_POINT ( 'NONE',  ( -73.00000000000001421, 171.6227766016838245, -5.000000000000007994 ) ) ;
#1087 = CARTESIAN_POINT ( 'NONE',  ( -45.00000000000000000, 171.6227766016838245, 0.000000000000000000 ) ) ;
#1088 = DIRECTION ( 'NONE',  ( 0.000000000000000000, 0.000000000000000000, 1.000000000000000000 ) ) ;
#1089 = CARTESIAN_POINT ( 'NONE',  ( -13.45813206906208848, 31.92660440999782523, -10.88283926110020516 ) ) ;
#1090 = ORIENTED_EDGE ( 'NONE', *, *, #11674, .T. ) ;
#1091 = DIRECTION ( 'NONE',  ( 0.000000000000000000, 0.8660254037844363761, 0.5000000000000039968 ) ) ;
#1092 = AXIS2_PLACEMENT_3D ( 'NONE', #293, #5694, #5962 ) ;
#1093 = ORIENTED_EDGE ( 'NONE', *, *, #6614, .F. ) ;
#1094 = EDGE_CURVE ( 'NONE', #9959, #11327, #2634, .T. ) ;
#1095 = CARTESIAN_POINT ( 'NONE',  ( 24.58901960448729085, 194.0039740083362858, -26.91197613625888607 ) ) ;
#1096 = CIRCLE ( 'NONE', #12121, 750.0000000000001137 ) ;
#1097 = LINE ( 'NONE', #6676, #9215 ) ;
#1098 = ORIENTED_EDGE ( 'NONE', *, *, #4065, .F. ) ;
#1099 = ORIENTED_EDGE ( 'NONE', *, *, #6963, .F. ) ;
#1100 = VERTEX_POINT ( 'NONE', #10936 ) ;
#1101 = EDGE_CURVE ( 'NONE', #2967, #7107, #9049, .T. ) ;
#1102 = CARTESIAN_POINT ( 'NONE',  ( -87.44048204095830101, 147.5870804700067822, -22.61345334826514630 ) ) ;
#1103 = EDGE_CURVE ( 'NONE', #1074, #16221, #15014, .T. ) ;
#1104 = VECTOR ( 'NONE', #1505, 1000.000000000000000 ) ;
#1105 = ORIENTED_EDGE ( 'NONE', *, *, #4082, .F. ) ;
#1106 = CARTESIAN_POINT ( 'NONE',  ( 0.000000000000000000, 0.000000000000000000, 0.000000000000000000 ) ) ;
#1107 = VECTOR ( 'NONE', #12507, 1000.000000000000000 ) ;
#1108 = CARTESIAN_POINT ( 'NONE',  ( -12.31336727611479631, 31.57746213708666971, 11.68681022658133806 ) ) ;
#1109 = AXIS2_PLACEMENT_3D ( 'NONE', #12893, #768, #9885 ) ;
#1110 = SURFACE_STYLE_FILL_AREA ( #5093 ) ;
#1111 = CARTESIAN_POINT ( 'NONE',  ( 33.34658291204065250, 151.6073998100962399, -28.71242994986355868 ) ) ;
#1112 = CARTESIAN_POINT ( 'NONE',  ( 20.95008785553089581, 29.88049067427350280, 10.28044474760307914 ) ) ;
#1113 = CARTESIAN_POINT ( 'NONE',  ( -84.53126297072897444, 148.7415597018667199, 23.77993541092453000 ) ) ;
#1114 = ORIENTED_EDGE ( 'NONE', *, *, #6133, .T. ) ;
#1115 = DIRECTION ( 'NONE',  ( -1.000000000000000000, 0.000000000000000000, -8.673617379884037937E-17 ) ) ;
#1116 = CARTESIAN_POINT ( 'NONE',  ( 24.93507336697352628, 29.86842105263157876, -4.999999999999999112 ) ) ;
#1117 = LINE ( 'NONE', #9603, #8779 ) ;
#1118 = CARTESIAN_POINT ( 'NONE',  ( 17.55923266082603007, 17.99999999999999645, 24.87049340120105612 ) ) ;
#1119 = CARTESIAN_POINT ( 'NONE',  ( -17.89548297089572060, 32.23709896788771090, -7.636891392351368602 ) ) ;
#1120 = ORIENTED_EDGE ( 'NONE', *, *, #16638, .T. ) ;
#1121 = CARTESIAN_POINT ( 'NONE',  ( -77.50000000000002842, 146.6227766016838245, -16.00000000000000000 ) ) ;
#1122 = AXIS2_PLACEMENT_3D ( 'NONE', #1780, #8415, #7174 ) ;
#1123 = CIRCLE ( 'NONE', #11293, 33.00000000000000000 ) ;
#1124 = AXIS2_PLACEMENT_3D ( 'NONE', #7031, #4466, #16505 ) ;
#1125 = PRODUCT_RELATED_PRODUCT_CATEGORY ( 'part', '', ( #1782 ) ) ;
#1126 = FACE_OUTER_BOUND ( 'NONE', #11539, .T. ) ;
#1127 = ORIENTED_EDGE ( 'NONE', *, *, #12799, .F. ) ;
#1128 = CYLINDRICAL_SURFACE ( 'NONE', #12151, 2.499999999999998668 ) ;
#1129 = EDGE_CURVE ( 'NONE', #15972, #15553, #1392, .T. ) ;
#1130 = VERTEX_POINT ( 'NONE', #142 ) ;
#1131 = CARTESIAN_POINT ( 'NONE',  ( -100.0000000000000000, 201.6227766016838245, 0.000000000000000000 ) ) ;
#1132 = CARTESIAN_POINT ( 'NONE',  ( 19.47274266584701508, 18.00000000000000000, -24.48069943974689266 ) ) ;
#1133 = CARTESIAN_POINT ( 'NONE',  ( -74.13623385059629811, 145.1725333695280256, -22.94453145061436672 ) ) ;
#1134 = AXIS2_PLACEMENT_3D ( 'NONE', #14330, #2289, #13091 ) ;
#1135 = AXIS2_PLACEMENT_3D ( 'NONE', #9812, #3088, #5745 ) ;
#1136 = CARTESIAN_POINT ( 'NONE',  ( -34.99999999999999289, 130.0000000000000000, 15.00000000000000000 ) ) ;
#1137 = ORIENTED_EDGE ( 'NONE', *, *, #8044, .F. ) ;
#1138 = CARTESIAN_POINT ( 'NONE',  ( -103.0000000000000142, 171.6227766016838245, 0.000000000000000000 ) ) ;
#1139 = CARTESIAN_POINT ( 'NONE',  ( -206.6025269363104258, 173.6007587957575993, -4.555677747302790515 ) ) ;
#1140 = EDGE_CURVE ( 'NONE', #11894, #1799, #5659, .T. ) ;
#1141 = DIRECTION ( 'NONE',  ( -0.000000000000000000, -0.000000000000000000, -1.000000000000000000 ) ) ;
#1142 = ORIENTED_EDGE ( 'NONE', *, *, #11588, .F. ) ;
#1143 = EDGE_LOOP ( 'NONE', ( #15959, #17118, #14386, #12047, #15475, #7216, #8312 ) ) ;
#1144 = DIRECTION ( 'NONE',  ( -1.000000000000000000, -0.000000000000000000, -0.000000000000000000 ) ) ;
#1145 = ORIENTED_EDGE ( 'NONE', *, *, #11841, .F. ) ;
#1146 = CARTESIAN_POINT ( 'NONE',  ( -81.80240525860705247, 152.3499437555877591, -29.21584945930381139 ) ) ;
#1147 = CIRCLE ( 'NONE', #866, 24.99999999999999645 ) ;
#1148 = CARTESIAN_POINT ( 'NONE',  ( 14.24852413927196970, 138.7494242586804489, -7.288003809479805639 ) ) ;
#1149 = ORIENTED_EDGE ( 'NONE', *, *, #15369, .T. ) ;
#1150 = CARTESIAN_POINT ( 'NONE',  ( 34.93420767853316988, 18.00000000000000355, 0.000000000000000000 ) ) ;
#1151 = CARTESIAN_POINT ( 'NONE',  ( 49.99999999999998579, 163.6227766016838530, 12.50000337241049309 ) ) ;
#1152 = DIRECTION ( 'NONE',  ( -1.000000000000000000, -0.000000000000000000, -0.000000000000000000 ) ) ;
#1153 = DIRECTION ( 'NONE',  ( -1.000000000000000000, 0.000000000000000000, 0.000000000000000000 ) ) ;
#1154 = DIRECTION ( 'NONE',  ( 1.000000000000000000, 0.000000000000000000, 0.000000000000000000 ) ) ;
#1155 = DIRECTION ( 'NONE',  ( 0.000000000000000000, 1.000000000000000000, 0.000000000000000000 ) ) ;
#1156 = CARTESIAN_POINT ( 'NONE',  ( -74.00000000000002842, 146.6227766016838245, -24.49489742783179125 ) ) ;
#1157 = AXIS2_PLACEMENT_3D ( 'NONE', #9341, #15001, #16173 ) ;
#1158 = CARTESIAN_POINT ( 'NONE',  ( -16.30611068361784532, 32.76923076923076650, 4.999999999999998224 ) ) ;
#1159 = ADVANCED_FACE ( 'NONE', ( #4225 ), #17507, .T. ) ;
#1160 = EDGE_CURVE ( 'NONE', #5721, #668, #2888, .T. ) ;
#1161 = DIRECTION ( 'NONE',  ( -1.000000000000000000, -0.000000000000000000, 0.000000000000000000 ) ) ;
#1162 = EDGE_CURVE ( 'NONE', #12168, #12804, #12449, .T. ) ;
#1163 = CYLINDRICAL_SURFACE ( 'NONE', #14285, 2.500000000000000444 ) ;
#1164 = VERTEX_POINT ( 'NONE', #10039 ) ;
#1165 = LINE ( 'NONE', #11957, #3637 ) ;
#1166 = CARTESIAN_POINT ( 'NONE',  ( -24.80114670877660643, 19.99999999999999289, -15.70637264050929538 ) ) ;
#1167 = EDGE_LOOP ( 'NONE', ( #9373, #13594, #16037, #1479, #35, #4200 ) ) ;
#1168 = DIRECTION ( 'NONE',  ( -1.000000000000000000, 0.000000000000000000, 0.000000000000000000 ) ) ;
#1169 = CARTESIAN_POINT ( 'NONE',  ( 1.559999999999998943, -1.732050807568885631, 0.000000000000000000 ) ) ;
#1170 = VERTEX_POINT ( 'NONE', #2233 ) ;
#1171 = DIRECTION ( 'NONE',  ( -1.156482317317868274E-16, 1.000000000000000000, 0.000000000000000000 ) ) ;
#1172 = CARTESIAN_POINT ( 'NONE',  ( 18.85693063297101801, 142.3798671548016159, 15.29581099734062022 ) ) ;
#1173 = VERTEX_POINT ( 'NONE', #8548 ) ;
#1174 = CARTESIAN_POINT ( 'NONE',  ( -82.50000000000002842, 146.6227766016838245, -16.00000000000000000 ) ) ;
#1175 = ORIENTED_EDGE ( 'NONE', *, *, #17079, .T. ) ;
#1176 = CARTESIAN_POINT ( 'NONE',  ( -32.66708739526796279, 101.0000000000000142, 4.722170599040663497 ) ) ;
#1177 = CARTESIAN_POINT ( 'NONE',  ( 22.65282855708332121, 195.0632477915244181, -23.23525722188764675 ) ) ;
#1178 = CYLINDRICAL_SURFACE ( 'NONE', #9082, 2.500000000000000444 ) ;
#1179 = CARTESIAN_POINT ( 'NONE',  ( -12.51506868919167026, 18.00000000000000000, -7.695309128566540480 ) ) ;
#1180 = ORIENTED_EDGE ( 'NONE', *, *, #2081, .F. ) ;
#1181 = DIRECTION ( 'NONE',  ( -1.000000000000000000, -6.938893903907228378E-16, 0.000000000000000000 ) ) ;
#1182 = ORIENTED_EDGE ( 'NONE', *, *, #17382, .T. ) ;
#1183 = CARTESIAN_POINT ( 'NONE',  ( -74.54484354042847372, 191.4518784269448588, -26.38258506112510915 ) ) ;
#1184 = FACE_OUTER_BOUND ( 'NONE', #5191, .T. ) ;
#1185 = VERTEX_POINT ( 'NONE', #15776 ) ;
#1186 = ORIENTED_EDGE ( 'NONE', *, *, #14469, .T. ) ;
#1187 = EDGE_LOOP ( 'NONE', ( #2373, #9713, #10320, #7062, #15674, #5505, #13725, #7217, #5355, #10451, #13582, #2814 ) ) ;
#1188 = CARTESIAN_POINT ( 'NONE',  ( -86.35693927557340999, 150.6299487802827457, -25.46745035168473237 ) ) ;
#1189 = ORIENTED_EDGE ( 'NONE', *, *, #10276, .T. ) ;
#1190 = CARTESIAN_POINT ( 'NONE',  ( 0.000000000000000000, 0.000000000000000000, 0.000000000000000000 ) ) ;
#1191 = ADVANCED_FACE ( 'NONE', ( #911 ), #322, .T. ) ;
#1192 = CARTESIAN_POINT ( 'NONE',  ( 15.60228996707308191, 124.9392590765123998, -1.671679228207827439 ) ) ;
#1193 = EDGE_CURVE ( 'NONE', #16427, #7978, #1741, .T. ) ;
#1194 = DIRECTION ( 'NONE',  ( 0.000000000000000000, 0.000000000000000000, 1.000000000000000000 ) ) ;
#1195 = ADVANCED_FACE ( 'NONE', ( #4395 ), #492, .F. ) ;
#1196 = CARTESIAN_POINT ( 'NONE',  ( 32.20193699137669086, 152.2211730668986149, -29.13124974281948809 ) ) ;
#1197 = DIRECTION ( 'NONE',  ( 1.000000000000000000, 0.000000000000000000, 0.000000000000000000 ) ) ;
#1198 = CARTESIAN_POINT ( 'NONE',  ( -75.46486027377252981, 148.7497411309094844, 23.78985390322973714 ) ) ;
#1199 = VERTEX_POINT ( 'NONE', #3236 ) ;
#1200 = DIRECTION ( 'NONE',  ( 0.000000000000000000, 0.000000000000000000, -1.000000000000000000 ) ) ;
#1201 = DIRECTION ( 'NONE',  ( 1.000000000000000000, -0.000000000000000000, -0.000000000000000000 ) ) ;
#1202 = CARTESIAN_POINT ( 'NONE',  ( 17.39133856982844506, 125.9242906883583970, 6.521754810248964418 ) ) ;
#1203 = CARTESIAN_POINT ( 'NONE',  ( -87.50000000000004263, 146.6227766016838245, -21.54065922853802562 ) ) ;
#1204 = DIRECTION ( 'NONE',  ( -0.000000000000000000, -0.000000000000000000, 1.000000000000000000 ) ) ;
#1205 = EDGE_LOOP ( 'NONE', ( #1850, #12761, #371, #14836, #141 ) ) ;
#1206 = CARTESIAN_POINT ( 'NONE',  ( -87.43684327452987759, 145.5208630140649859, -20.20962120078074165 ) ) ;
#1207 = CARTESIAN_POINT ( 'NONE',  ( 29.50744102577957761, 201.5998317580112200, 13.79770299781523413 ) ) ;
#1208 = ORIENTED_EDGE ( 'NONE', *, *, #14941, .T. ) ;
#1209 = DIRECTION ( 'NONE',  ( -1.000000000000000000, 0.000000000000000000, 0.000000000000000000 ) ) ;
#1210 = CARTESIAN_POINT ( 'NONE',  ( 30.00000000000001066, 146.6227766016838245, -13.00000000000000000 ) ) ;
#1211 = EDGE_LOOP ( 'NONE', ( #16, #8549, #7703 ) ) ;
#1212 = PRESENTATION_STYLE_ASSIGNMENT (( #2453 ) ) ;
#1213 = DIRECTION ( 'NONE',  ( -0.08715574274765344742, -0.4980973490458779906, 0.8627299156628184251 ) ) ;
#1214 = ADVANCED_FACE ( 'NONE', ( #11195 ), #11869, .T. ) ;
#1215 = AXIS2_PLACEMENT_3D ( 'NONE', #10912, #3879, #6436 ) ;
#1216 = CARTESIAN_POINT ( 'NONE',  ( 17.53546816055560953, 18.00000000000000000, -24.87355917367171187 ) ) ;
#1217 = CARTESIAN_POINT ( 'NONE',  ( -76.83884856045256129, 141.5060039278119177, -17.83622402891603542 ) ) ;
#1218 = CARTESIAN_POINT ( 'NONE',  ( -12.63167751028161589, 20.00000000000000355, 24.35243221814332060 ) ) ;
#1219 = VERTEX_POINT ( 'NONE', #8634 ) ;
#1220 = CARTESIAN_POINT ( 'NONE',  ( -40.00000000000000000, 4.000000000000000000, 30.00000000000000711 ) ) ;
#1221 = EDGE_CURVE ( 'NONE', #10037, #12789, #8487, .T. ) ;
#1222 = DIRECTION ( 'NONE',  ( 0.000000000000000000, 0.000000000000000000, -1.000000000000000000 ) ) ;
#1223 = DIRECTION ( 'NONE',  ( 0.000000000000000000, 0.000000000000000000, 1.000000000000000000 ) ) ;
#1224 = ADVANCED_FACE ( 'NONE', ( #3655 ), #8591, .T. ) ;
#1225 = FACE_OUTER_BOUND ( 'NONE', #4522, .T. ) ;
#1226 = EDGE_CURVE ( 'NONE', #3871, #7408, #17464, .T. ) ;
#1227 = VERTEX_POINT ( 'NONE', #10461 ) ;
#1228 = CARTESIAN_POINT ( 'NONE',  ( 10.91733900447607830, 142.2434614804602404, -19.02291218241819593 ) ) ;
#1229 = ORIENTED_EDGE ( 'NONE', *, *, #5759, .T. ) ;
#1230 = LINE ( 'NONE', #13183, #8950 ) ;
#1231 = CARTESIAN_POINT ( 'NONE',  ( 14.60960092688903700, 138.5353766997065179, -5.001077596136161318 ) ) ;
#1232 = ORIENTED_EDGE ( 'NONE', *, *, #3927, .T. ) ;
#1233 = EDGE_CURVE ( 'NONE', #8974, #10007, #14992, .T. ) ;
#1234 = CARTESIAN_POINT ( 'NONE',  ( 49.99999999999998579, 183.6227766016837961, 5.571800142134975431 ) ) ;
#1235 = FACE_OUTER_BOUND ( 'NONE', #1413, .T. ) ;
#1236 = DIRECTION ( 'NONE',  ( 1.000000000000000000, 0.000000000000000000, -0.000000000000000000 ) ) ;
#1237 = CARTESIAN_POINT ( 'NONE',  ( -38.00000000000000000, 2.000000000000000000, 0.000000000000000000 ) ) ;
#1238 = LINE ( 'NONE', #9294, #4157 ) ;
#1239 = CARTESIAN_POINT ( 'NONE',  ( 17.13110662433428288, 29.95577564710725227, -12.69327266642979168 ) ) ;
#1240 = DIRECTION ( 'NONE',  ( 1.000000000000000000, -0.000000000000000000, -0.000000000000000000 ) ) ;
#1241 = DIRECTION ( 'NONE',  ( -1.000000000000000000, -0.000000000000000000, 0.000000000000000000 ) ) ;
#1242 = DIRECTION ( 'NONE',  ( 0.000000000000000000, 0.000000000000000000, 1.000000000000000000 ) ) ;
#1243 = DIRECTION ( 'NONE',  ( -1.000000000000000000, -0.000000000000000000, 0.000000000000000000 ) ) ;
#1244 = VECTOR ( 'NONE', #791, 1000.000000000000000 ) ;
#1245 = VERTEX_POINT ( 'NONE', #7094 ) ;
#1246 = CARTESIAN_POINT ( 'NONE',  ( 17.51892952578853979, 125.6677330052578014, -5.783603459598163354 ) ) ;
#1247 = ORIENTED_EDGE ( 'NONE', *, *, #8739, .F. ) ;
#1248 = DIRECTION ( 'NONE',  ( 1.000000000000000000, 0.000000000000000000, 0.000000000000000000 ) ) ;
#1249 = CARTESIAN_POINT ( 'NONE',  ( -40.00000000000000000, 0.000000000000000000, 30.00000000000000355 ) ) ;
#1250 = VERTEX_POINT ( 'NONE', #13649 ) ;
#1251 = CARTESIAN_POINT ( 'NONE',  ( -10.84365596476886395, 30.77158821550125722, 14.49076147631418721 ) ) ;
#1252 = CARTESIAN_POINT ( 'NONE',  ( 15.56337975240378846, 125.2134999403455851, 5.000000000000001776 ) ) ;
#1253 = ADVANCED_FACE ( 'NONE', ( #4444 ), #13571, .T. ) ;
#1254 = ORIENTED_EDGE ( 'NONE', *, *, #6754, .F. ) ;
#1255 = EDGE_CURVE ( 'NONE', #4882, #15354, #16487, .T. ) ;
#1256 = CARTESIAN_POINT ( 'NONE',  ( -43.00000000000000000, 140.0000000000000000, -15.00000000000000000 ) ) ;
#1257 = EDGE_CURVE ( 'NONE', #4434, #6774, #2765, .T. ) ;
#1258 = AXIS2_PLACEMENT_3D ( 'NONE', #13743, #7018, #2858 ) ;
#1259 = EDGE_LOOP ( 'NONE', ( #12011, #13058, #12458, #11892 ) ) ;
#1260 = AXIS2_PLACEMENT_3D ( 'NONE', #15232, #14882, #16485 ) ;
#1261 = DIRECTION ( 'NONE',  ( -1.000000000000000000, 0.000000000000000000, 0.000000000000000000 ) ) ;
#1262 = CARTESIAN_POINT ( 'NONE',  ( -208.1430079281944074, 176.3671987152221448, 3.647967993167786194 ) ) ;
#1263 = CARTESIAN_POINT ( 'NONE',  ( 34.99999999999999289, -20.00000000000000000, -35.00000000000002132 ) ) ;
#1264 = CARTESIAN_POINT ( 'NONE',  ( -12.79675654462651124, 17.99999999999533529, -5.581853174322293221 ) ) ;
#1265 = ORIENTED_EDGE ( 'NONE', *, *, #4152, .T. ) ;
#1266 = CARTESIAN_POINT ( 'NONE',  ( 31.88903224608757014, 151.2561509761041521, 25.96550485207007242 ) ) ;
#1267 = ORIENTED_EDGE ( 'NONE', *, *, #10879, .F. ) ;
#1268 = CARTESIAN_POINT ( 'NONE',  ( -5.000000000000000888, 154.3022685259950038, -9.999999999999900524 ) ) ;
#1269 = CARTESIAN_POINT ( 'NONE',  ( 6.134011831684059501, 134.2062027339443944, 24.99999999999999645 ) ) ;
#1270 = AXIS2_PLACEMENT_3D ( 'NONE', #12415, #2602, #285 ) ;
#1271 = VECTOR ( 'NONE', #13608, 1000.000000000000000 ) ;
#1272 = ORIENTED_EDGE ( 'NONE', *, *, #5599, .F. ) ;
#1273 = VECTOR ( 'NONE', #10193, 1000.000000000000000 ) ;
#1274 = ORIENTED_EDGE ( 'NONE', *, *, #7864, .F. ) ;
#1275 = ORIENTED_EDGE ( 'NONE', *, *, #16170, .T. ) ;
#1276 = ADVANCED_FACE ( 'NONE', ( #8318 ), #3109, .F. ) ;
#1277 = DIRECTION ( 'NONE',  ( 0.000000000000000000, 0.000000000000000000, -1.000000000000000000 ) ) ;
#1278 = EDGE_CURVE ( 'NONE', #16623, #14931, #1441, .T. ) ;
#1279 = VERTEX_POINT ( 'NONE', #9735 ) ;
#1280 = PRODUCT_CONTEXT ( 'NONE', #3711, 'mechanical' ) ;
#1281 = DIRECTION ( 'NONE',  ( 0.000000000000000000, 0.000000000000000000, 1.000000000000000000 ) ) ;
#1282 = PLANE ( 'NONE',  #4700 ) ;
#1283 = AXIS2_PLACEMENT_3D ( 'NONE', #13329, #1194, #11989 ) ;
#1284 = CARTESIAN_POINT ( 'NONE',  ( 30.00000000000000355, 196.6227766016838245, 1.387778780781445676E-14 ) ) ;
#1285 = CARTESIAN_POINT ( 'NONE',  ( -45.00000000000000000, 142.5209969267753820, -19.44444444444444997 ) ) ;
#1286 = CARTESIAN_POINT ( 'NONE',  ( -27.98221281347037959, 18.00000000000000355, -4.999999999999999112 ) ) ;
#1287 = CIRCLE ( 'NONE', #12024, 33.00000000000000000 ) ;
#1288 = ORIENTED_EDGE ( 'NONE', *, *, #2762, .F. ) ;
#1289 = CARTESIAN_POINT ( 'NONE',  ( -95.00000000000000000, 141.6227766016838245, -5.510910596163088767E-15 ) ) ;
#1290 = AXIS2_PLACEMENT_3D ( 'NONE', #12383, #12474, #5403 ) ;
#1291 = CARTESIAN_POINT ( 'NONE',  ( 23.92262868871285519, 29.88142130320016676, -9.432657661123421633 ) ) ;
#1292 = CARTESIAN_POINT ( 'NONE',  ( 15.65639489742288681, 128.1581396164810940, 10.28488489824641761 ) ) ;
#1293 = CARTESIAN_POINT ( 'NONE',  ( 24.94691999498327206, 18.00000000000000711, 22.32501294936691139 ) ) ;
#1294 = ORIENTED_EDGE ( 'NONE', *, *, #176, .T. ) ;
#1295 = DIRECTION ( 'NONE',  ( -1.000000000000000000, 0.000000000000000000, 0.000000000000000000 ) ) ;
#1296 = EDGE_CURVE ( 'NONE', #457, #14780, #101, .T. ) ;
#1297 = STYLED_ITEM ( 'NONE', ( #15804 ), #5484 ) ;
#1298 = CARTESIAN_POINT ( 'NONE',  ( -82.50000000000002842, 146.6227766016838245, -16.00000000000000000 ) ) ;
#1299 = DIRECTION ( 'NONE',  ( -1.000000000000000000, 0.000000000000000000, 0.000000000000000000 ) ) ;
#1300 = AXIS2_PLACEMENT_3D ( 'NONE', #2966, #10847, #2802 ) ;
#1301 = VERTEX_POINT ( 'NONE', #12231 ) ;
#1302 = CYLINDRICAL_SURFACE ( 'NONE', #11228, 3.999999999999999556 ) ;
#1303 = EDGE_LOOP ( 'NONE', ( #11441, #8846, #10583, #13960 ) ) ;
#1304 = CARTESIAN_POINT ( 'NONE',  ( -208.0000000000000853, 170.0678595944000620, 2.693195258168412654 ) ) ;
#1305 = CARTESIAN_POINT ( 'NONE',  ( -40.00000000000000000, 4.000000000000000000, 33.00000000000000711 ) ) ;
#1306 = B_SPLINE_CURVE_WITH_KNOTS ( 'NONE', 3,
 ( #17039, #4907, #5174, #10296, #4835, #9065, #15703, #11713, #2423, #13325, #6594, #7824, #13232, #6243, #10563, #6410, #6316, #2255, #17120, #8977, #3584, #9240, #15623, #15796, #2165, #11985, #7651, #14388, #9146, #2338, #10223, #4997, #14552, #17304, #13061, #927, #1188, #3679, #14474, #7728, #13138, #1102, #1006, #3498, #8886, #11804 ),
 .UNSPECIFIED., .F., .F.,
 ( 4, 2, 2, 2, 2, 2, 2, 2, 2, 2, 2, 2, 2, 2, 2, 2, 2, 2, 2, 2, 2, 2, 4 ),
 ( 0.01035378412632265675, 0.01206629175607497849, 0.01377879938582729849, 0.01549130701557962023, 0.01634756083045581232, 0.01720381464533200441, 0.01806006846020819651, 0.01891632227508438860, 0.02062882990483675544, 0.02148508371971293712, 0.02234133753458911881, 0.02319759134946530049, 0.02405384516434148218, 0.02576635279409380738, 0.02747886042384612565, 0.02833511423872230733, 0.02919136805359848902, 0.03090387568335084545, 0.03261638331310320188, 0.03432889094285555831, 0.03604139857260792168, 0.03689765238748409643, 0.03775390620236027117 ),
 .UNSPECIFIED. ) ;
#1307 = CARTESIAN_POINT ( 'NONE',  ( -83.14994314962653732, 141.4992599418080488, -17.82476597062853685 ) ) ;
#1308 = DIRECTION ( 'NONE',  ( 0.000000000000000000, 0.000000000000000000, 1.000000000000000000 ) ) ;
#1309 = CIRCLE ( 'NONE', #7792, 6.000000000000005329 ) ;
#1310 = VERTEX_POINT ( 'NONE', #4270 ) ;
#1311 = DIRECTION ( 'NONE',  ( 1.000000000000000000, 0.000000000000000000, 0.000000000000000000 ) ) ;
#1312 = CARTESIAN_POINT ( 'NONE',  ( 25.49999999999998579, 9.999999999999998224, 0.000000000000000000 ) ) ;
#1313 = DIRECTION ( 'NONE',  ( 1.000000000000000000, 0.000000000000000000, 0.000000000000000000 ) ) ;
#1314 = CYLINDRICAL_SURFACE ( 'NONE', #2976, 250.0000000000000000 ) ;
#1315 = ADVANCED_FACE ( 'NONE', ( #11245 ), #361, .F. ) ;
#1316 = ORIENTED_EDGE ( 'NONE', *, *, #2532, .T. ) ;
#1317 = CARTESIAN_POINT ( 'NONE',  ( 15.14881438696876614, 128.6905335926829252, -10.89137921944116449 ) ) ;
#1318 = EDGE_CURVE ( 'NONE', #10436, #10138, #2839, .T. ) ;
#1319 = ORIENTED_EDGE ( 'NONE', *, *, #6992, .F. ) ;
#1320 = CARTESIAN_POINT ( 'NONE',  ( -78.88444202303340091, 152.5224481282687066, -29.32884290898093838 ) ) ;
#1321 = VECTOR ( 'NONE', #8240, 1000.000000000000000 ) ;
#1322 = CARTESIAN_POINT ( 'NONE',  ( 12.89436750745977989, 143.6582566230365501, -17.52127501928458031 ) ) ;
#1323 = VECTOR ( 'NONE', #16410, 1000.000000000000000 ) ;
#1324 = ORIENTED_EDGE ( 'NONE', *, *, #2716, .F. ) ;
#1325 = DIRECTION ( 'NONE',  ( 0.000000000000000000, 0.000000000000000000, 1.000000000000000000 ) ) ;
#1326 = AXIS2_PLACEMENT_3D ( 'NONE', #7125, #1990, #12349 ) ;
#1327 = DIRECTION ( 'NONE',  ( -0.000000000000000000, -0.000000000000000000, -1.000000000000000000 ) ) ;
#1328 = EDGE_CURVE ( 'NONE', #7719, #846, #9653, .T. ) ;
#1329 = EDGE_CURVE ( 'NONE', #16720, #11161, #11838, .T. ) ;
#1330 = AXIS2_PLACEMENT_3D ( 'NONE', #4533, #1952, #4869 ) ;
#1331 = DIRECTION ( 'NONE',  ( 0.000000000000000000, 0.000000000000000000, 1.000000000000000000 ) ) ;
#1332 = APPLICATION_CONTEXT ( 'automotive_design' ) ;
#1333 = DIRECTION ( 'NONE',  ( -0.000000000000000000, -0.000000000000000000, -1.000000000000000000 ) ) ;
#1334 = CARTESIAN_POINT ( 'NONE',  ( 19.49710218362280045, 17.99999999999999289, -24.48336163992366465 ) ) ;
#1335 = CARTESIAN_POINT ( 'NONE',  ( 20.28823715622366919, 18.00000000000000000, -11.10707270023369730 ) ) ;
#1336 = CARTESIAN_POINT ( 'NONE',  ( -71.66708739526794147, 110.0000000000000142, -4.499999999999999112 ) ) ;
#1337 = DIRECTION ( 'NONE',  ( -0.000000000000000000, -0.000000000000000000, -1.000000000000000000 ) ) ;
#1338 = CARTESIAN_POINT ( 'NONE',  ( -40.00000000000000000, 8.000000000000007105, 30.00000000000000355 ) ) ;
#1339 = AXIS2_PLACEMENT_3D ( 'NONE', #16014, #2207, #14432 ) ;
#1340 = CARTESIAN_POINT ( 'NONE',  ( 27.40214814073310023, 141.2103550623191381, -17.32402235562967263 ) ) ;
#1341 = ORIENTED_EDGE ( 'NONE', *, *, #12280, .F. ) ;
#1342 = DIRECTION ( 'NONE',  ( 0.000000000000000000, 0.000000000000000000, 1.000000000000000000 ) ) ;
#1343 = VECTOR ( 'NONE', #4860, 1000.000000000000000 ) ;
#1344 = ORIENTED_EDGE ( 'NONE', *, *, #16537, .T. ) ;
#1345 = COLOUR_RGB ( '', 0.08235294, 0.09019608, 0.10196078) ;
#1346 = CARTESIAN_POINT ( 'NONE',  ( 48.00000000000000711, 179.6227766016838245, -15.00000337241049486 ) ) ;
#1347 = STYLED_ITEM ( 'NONE', ( #12882 ), #17066 ) ;
#1348 = LINE ( 'NONE', #12051, #466 ) ;
#1349 = VERTEX_POINT ( 'NONE', #6910 ) ;
#1350 = CARTESIAN_POINT ( 'NONE',  ( -12.14981508666162036, 19.99999999999543121, 12.53017279448777366 ) ) ;
#1351 = PRODUCT_DEFINITION ( 'UNKNOWN', '', #8975, #12448 ) ;
#1352 = DIRECTION ( 'NONE',  ( 1.000000000000000000, 0.000000000000000000, 0.000000000000000000 ) ) ;
#1353 = ORIENTED_EDGE ( 'NONE', *, *, #8803, .T. ) ;
#1354 = DIRECTION ( 'NONE',  ( 0.000000000000000000, 0.000000000000000000, 1.000000000000000000 ) ) ;
#1355 = ORIENTED_EDGE ( 'NONE', *, *, #6344, .T. ) ;
#1356 = CYLINDRICAL_SURFACE ( 'NONE', #8665, 27.69059892324149530 ) ;
#1357 = CARTESIAN_POINT ( 'NONE',  ( 37.49298393897301196, 196.2445469595302825, -21.97388680505722292 ) ) ;
#1358 = CARTESIAN_POINT ( 'NONE',  ( 17.58250999373989742, 125.2198453306090045, -1.666666666666656749 ) ) ;
#1359 = DIRECTION ( 'NONE',  ( -1.000000000000000000, 0.000000000000000000, 0.000000000000000000 ) ) ;
#1360 = ORIENTED_EDGE ( 'NONE', *, *, #6788, .T. ) ;
#1361 = CARTESIAN_POINT ( 'NONE',  ( 29.00744693363358806, 151.5270838226223873, 26.17568438743891335 ) ) ;
#1362 = EDGE_CURVE ( 'NONE', #10642, #15641, #16945, .T. ) ;
#1363 = ORIENTED_EDGE ( 'NONE', *, *, #15702, .F. ) ;
#1364 = CARTESIAN_POINT ( 'NONE',  ( -83.07446265461977930, 189.7763206329742331, -27.55849099911373656 ) ) ;
#1365 = DIRECTION ( 'NONE',  ( -1.000000000000000000, 0.000000000000000000, 0.000000000000000000 ) ) ;
#1366 =( BOUNDED_SURFACE ( )  B_SPLINE_SURFACE ( 3, 2, ( 
 ( #1877, #551, #4626 ),
 ( #10001, #15412, #17087 ),
 ( #2309, #9116, #15760 ),
 ( #11605, #6287, #725 ),
 ( #7615, #12844, #11514 ),
 ( #11678, #5050, #3550 ),
 ( #14188, #814, #12937 ),
 ( #6032, #8935, #7699 ),
 ( #13106, #15505, #13029 ),
 ( #3382, #11426, #973 ),
 ( #6373, #11768, #10352 ),
 ( #15857, #14350, #900 ),
 ( #2049, #16835, #7528 ),
 ( #16926, #3642, #6208 ),
 ( #3730, #2127, #17011 ),
 ( #10266, #4959, #4877 ),
 ( #9032, #639, #8853 ),
 ( #4707, #17178, #10190 ),
 ( #14261, #2218, #10448 ),
 ( #14443, #4798, #1963 ),
 ( #7367, #15668, #15591 ),
 ( #12768, #10097, #3466 ),
 ( #7442, #8780, #6118 ),
 ( #13374, #13554, #1158 ) ),
 .UNSPECIFIED., .F., .F., .F. ) 
 B_SPLINE_SURFACE_WITH_KNOTS ( ( 4, 2, 2, 2, 2, 2, 2, 2, 2, 2, 2, 4 ),
 ( 3, 3 ),
 ( 0.01427588378380421734, 0.01824401167166928364, 0.02022807561560181766, 0.02221213955953435168, 0.02618026744739941625, 0.02816433139133195027, 0.03014839533526448428, 0.03411652322312955232, 0.03610058716706208287, 0.03808465111099461342, 0.04205277899885968146, 0.04602090688672474950 ),
 ( 0.000000000000000000, 1.000000000000000000 ),
 .UNSPECIFIED. ) 
 GEOMETRIC_REPRESENTATION_ITEM ( )  RATIONAL_B_SPLINE_SURFACE ( (
 ( 1.000000000000000000, 0.7071067811865476838, 1.000000000000000000),
 ( 1.000000000000000000, 0.7013659285812973154, 1.000000000000000000),
 ( 1.000000000000000000, 0.6957352470445186121, 1.000000000000000000),
 ( 1.000000000000000000, 0.6874449304734518984, 1.000000000000000000),
 ( 1.000000000000000000, 0.6847075230360146758, 1.000000000000000000),
 ( 1.000000000000000000, 0.6792848743381181276, 1.000000000000000000),
 ( 1.000000000000000000, 0.6765866164120997173, 1.000000000000000000),
 ( 1.000000000000000000, 0.6687223666255138754, 1.000000000000000000),
 ( 1.000000000000000000, 0.6637534122519734847, 1.000000000000000000),
 ( 1.000000000000000000, 0.6567012635109988894, 1.000000000000000000),
 ( 1.000000000000000000, 0.6544178910916050862, 1.000000000000000000),
 ( 1.000000000000000000, 0.6499901663948596253, 1.000000000000000000),
 ( 1.000000000000000000, 0.6478648508490586488, 1.000000000000000000),
 ( 1.000000000000000000, 0.6418284244075036504, 1.000000000000000000),
 ( 1.000000000000000000, 0.6382188548936987837, 1.000000000000000000),
 ( 1.000000000000000000, 0.6334349500989925330, 1.000000000000000000),
 ( 1.000000000000000000, 0.6319385063093012622, 1.000000000000000000),
 ( 1.000000000000000000, 0.6292162870120669993, 1.000000000000000000),
 ( 1.000000000000000000, 0.6279881568153810045, 1.000000000000000000),
 ( 1.000000000000000000, 0.6246939197237914021, 1.000000000000000000),
 ( 1.000000000000000000, 0.6230139244306683866, 1.000000000000000000),
 ( 1.000000000000000000, 0.6207349535630238835, 1.000000000000000000),
 ( 1.000000000000000000, 0.6201739322038456459, 1.000000000000000000),
 ( 1.000000000000000000, 0.6201736729460424202, 1.000000000000000000) ) ) 
 REPRESENTATION_ITEM ( '' )  SURFACE ( )  );
#1367 = VERTEX_POINT ( 'NONE', #16311 ) ;
#1368 = AXIS2_PLACEMENT_3D ( 'NONE', #14284, #2415, #6495 ) ;
#1369 = ORIENTED_EDGE ( 'NONE', *, *, #3514, .F. ) ;
#1370 = EDGE_LOOP ( 'NONE', ( #2054, #9589, #12874, #6617, #1090, #12711, #3516 ) ) ;
#1371 = AXIS2_PLACEMENT_3D ( 'NONE', #16024, #7965, #9288 ) ;
#1372 = STYLED_ITEM ( 'NONE', ( #12556 ), #2569 ) ;
#1373 = CARTESIAN_POINT ( 'NONE',  ( 12.56741672263968290, 142.0153054307823481, 18.66563201629009328 ) ) ;
#1374 = ORIENTED_EDGE ( 'NONE', *, *, #14927, .T. ) ;
#1375 = APPLICATION_PROTOCOL_DEFINITION ( 'draft international standard', 'automotive_design', 1998, #15236 ) ;
#1376 = CARTESIAN_POINT ( 'NONE',  ( 48.00000000000000000, 171.6227766016838245, -12.50000337241049131 ) ) ;
#1377 = DIRECTION ( 'NONE',  ( 0.000000000000000000, 0.000000000000000000, -1.000000000000000000 ) ) ;
#1378 = CYLINDRICAL_SURFACE ( 'NONE', #9581, 7.500000000000020428 ) ;
#1379 = DIRECTION ( 'NONE',  ( 0.000000000000000000, 1.000000000000000000, 0.000000000000000000 ) ) ;
#1380 = DIRECTION ( 'NONE',  ( 0.000000000000000000, 0.000000000000000000, -1.000000000000000000 ) ) ;
#1381 = AXIS2_PLACEMENT_3D ( 'NONE', #2085, #3164, #6248 ) ;
#1382 = ORIENTED_EDGE ( 'NONE', *, *, #14861, .F. ) ;
#1383 = CARTESIAN_POINT ( 'NONE',  ( -85.95768757437879515, 197.3572491277162726, -23.72357542124677110 ) ) ;
#1384 = EDGE_CURVE ( 'NONE', #12997, #2044, #3662, .T. ) ;
#1385 = EDGE_CURVE ( 'NONE', #8108, #13207, #13001, .T. ) ;
#1386 = DIRECTION ( 'NONE',  ( -1.000000000000000000, -0.000000000000000000, 0.000000000000000000 ) ) ;
#1387 = EDGE_CURVE ( 'NONE', #6730, #17412, #1609, .T. ) ;
#1388 = CARTESIAN_POINT ( 'NONE',  ( 14.93242934743711992, 18.00000000000000355, 25.00000000000000000 ) ) ;
#1389 = CARTESIAN_POINT ( 'NONE',  ( -80.00000000000002842, 146.6227766016838245, -16.00000000000000000 ) ) ;
#1390 = FACE_OUTER_BOUND ( 'NONE', #16381, .T. ) ;
#1391 = AXIS2_PLACEMENT_3D ( 'NONE', #9461, #9297, #14520 ) ;
#1392 = LINE ( 'NONE', #8368, #6804 ) ;
#1393 = AXIS2_PLACEMENT_3D ( 'NONE', #396, #7302, #5984 ) ;
#1394 = ORIENTED_EDGE ( 'NONE', *, *, #564, .T. ) ;
#1395 = CYLINDRICAL_SURFACE ( 'NONE', #17169, 2.499999999999998668 ) ;
#1396 = AXIS2_PLACEMENT_3D ( 'NONE', #9053, #831, #17027 ) ;
#1397 = ORIENTED_EDGE ( 'NONE', *, *, #15063, .T. ) ;
#1398 =( LENGTH_UNIT ( ) NAMED_UNIT ( * ) SI_UNIT ( .MILLI., .METRE. ) );
#1399 = CARTESIAN_POINT ( 'NONE',  ( -85.00000000000007105, 146.0036328918051254, 20.82208359987473401 ) ) ;
#1400 = DIRECTION ( 'NONE',  ( 1.000000000000000000, 0.000000000000000000, -1.445602896647339163E-16 ) ) ;
#1401 = ADVANCED_FACE ( 'NONE', ( #15134 ), #11070, .F. ) ;
#1402 = DIRECTION ( 'NONE',  ( -1.000000000000000000, 0.000000000000000000, 0.000000000000000000 ) ) ;
#1403 = ORIENTED_EDGE ( 'NONE', *, *, #4744, .T. ) ;
#1404 = FACE_OUTER_BOUND ( 'NONE', #12164, .T. ) ;
#1405 = CIRCLE ( 'NONE', #11292, 2.499999999999998668 ) ;
#1406 = AXIS2_PLACEMENT_3D ( 'NONE', #10309, #6169, #7577 ) ;
#1407 = DIRECTION ( 'NONE',  ( -2.674902700537819740E-31, 2.312964634635742267E-15, 1.000000000000000000 ) ) ;
#1408 = CIRCLE ( 'NONE', #2527, 2.500000000000000444 ) ;
#1409 = CARTESIAN_POINT ( 'NONE',  ( 27.99999999999998224, 9.999999999999998224, -35.00200000000000244 ) ) ;
#1410 = AXIS2_PLACEMENT_3D ( 'NONE', #3038, #15340, #566 ) ;
#1411 = CARTESIAN_POINT ( 'NONE',  ( -27.99999999999998224, 10.00000000000000000, -13.00000000000000000 ) ) ;
#1412 = CARTESIAN_POINT ( 'NONE',  ( 14.69130379018311316, 137.7259585328908713, -10.44822943247861247 ) ) ;
#1413 = EDGE_LOOP ( 'NONE', ( #9423, #8176 ) ) ;
#1414 = CARTESIAN_POINT ( 'NONE',  ( 48.00000000000000000, 171.6227766016838245, 0.000000000000000000 ) ) ;
#1415 = CARTESIAN_POINT ( 'NONE',  ( 15.45419697039644902, 125.5863960662987040, -6.086967932831932160 ) ) ;
#1416 = AXIS2_PLACEMENT_3D ( 'NONE', #3060, #15359, #11113 ) ;
#1417 = CONICAL_SURFACE ( 'NONE', #5376, 1732.050807568857181, 1.047197551196592746 ) ;
#1418 = ORIENTED_EDGE ( 'NONE', *, *, #10636, .F. ) ;
#1419 =( NAMED_UNIT ( * ) PLANE_ANGLE_UNIT ( ) SI_UNIT ( $, .RADIAN. ) );
#1420 = CYLINDRICAL_SURFACE ( 'NONE', #11309, 2.499999999999998668 ) ;
#1421 = CARTESIAN_POINT ( 'NONE',  ( 48.00000000000000711, 159.6227766016838814, -3.071800142134975431 ) ) ;
#1422 = EDGE_CURVE ( 'NONE', #6189, #8470, #2253, .T. ) ;
#1423 = DIRECTION ( 'NONE',  ( 0.000000000000000000, -0.000000000000000000, 1.000000000000000000 ) ) ;
#1424 = EDGE_CURVE ( 'NONE', #8476, #8508, #15662, .T. ) ;
#1425 = CARTESIAN_POINT ( 'NONE',  ( 25.51458778375578973, 18.00000000000000000, -21.98440010584615578 ) ) ;
#1426 = CARTESIAN_POINT ( 'NONE',  ( 19.16009641331746849, 29.91553747150882359, -11.79770956048753838 ) ) ;
#1427 = FACE_OUTER_BOUND ( 'NONE', #12569, .T. ) ;
#1428 = CYLINDRICAL_SURFACE ( 'NONE', #7596, 4.999999999999997335 ) ;
#1429 = PLANE ( 'NONE',  #14696 ) ;
#1430 = CARTESIAN_POINT ( 'NONE',  ( 28.01299615403722143, 140.9569246592376999, -16.87109569490920791 ) ) ;
#1431 = ORIENTED_EDGE ( 'NONE', *, *, #12069, .F. ) ;
#1432 = LINE ( 'NONE', #14963, #6757 ) ;
#1433 = VECTOR ( 'NONE', #8200, 1000.000000000000000 ) ;
#1434 = CIRCLE ( 'NONE', #13308, 5.000000000000007994 ) ;
#1435 = EDGE_LOOP ( 'NONE', ( #16840, #13854, #4027, #12176 ) ) ;
#1436 = CARTESIAN_POINT ( 'NONE',  ( 37.99999999999998579, 20.00000000000000000, 30.00000000000001066 ) ) ;
#1437 = CONICAL_SURFACE ( 'NONE', #13880, 2.499999999999998668, 1.029744260000002187 ) ;
#1438 = EDGE_CURVE ( 'NONE', #1227, #11461, #1405, .T. ) ;
#1439 = ORIENTED_EDGE ( 'NONE', *, *, #968, .T. ) ;
#1440 = DIRECTION ( 'NONE',  ( 1.000000000000000000, 0.000000000000000000, 0.000000000000000000 ) ) ;
#1441 = LINE ( 'NONE', #10982, #5955 ) ;
#1442 = ORIENTED_EDGE ( 'NONE', *, *, #3814, .T. ) ;
#1443 = CARTESIAN_POINT ( 'NONE',  ( 22.55951795904177004, 147.5870804700066685, -22.61345334826511078 ) ) ;
#1444 = CIRCLE ( 'NONE', #11332, 5.000000000000004441 ) ;
#1445 = VERTEX_POINT ( 'NONE', #11509 ) ;
#1446 = FACE_OUTER_BOUND ( 'NONE', #3207, .T. ) ;
#1447 = CARTESIAN_POINT ( 'NONE',  ( -23.00000000000002132, 100.0000000000000142, -4.999999999999999112 ) ) ;
#1448 = CARTESIAN_POINT ( 'NONE',  ( 17.54349574104648823, 125.4948194589026684, -4.999999999999997335 ) ) ;
#1449 = ORIENTED_EDGE ( 'NONE', *, *, #16449, .F. ) ;
#1450 = CARTESIAN_POINT ( 'NONE',  ( 27.75000000000000000, 0.000000000000000000, 0.000000000000000000 ) ) ;
#1451 = ORIENTED_EDGE ( 'NONE', *, *, #15961, .F. ) ;
#1452 = CARTESIAN_POINT ( 'NONE',  ( -45.00000000000000000, 120.0000000000000142, 15.00000000000000000 ) ) ;
#1453 = ORIENTED_EDGE ( 'NONE', *, *, #6083, .T. ) ;
#1454 = EDGE_CURVE ( 'NONE', #12318, #9593, #272, .T. ) ;
#1455 = CARTESIAN_POINT ( 'NONE',  ( -40.00000000000000000, 4.000000000000000000, -33.00000000000000711 ) ) ;
#1456 = CARTESIAN_POINT ( 'NONE',  ( -38.00000000000000000, 2.000000000000000000, 28.00000000000000355 ) ) ;
#1457 = EDGE_CURVE ( 'NONE', #1773, #6476, #6026, .T. ) ;
#1458 = VECTOR ( 'NONE', #4893, 1000.000000000000000 ) ;
#1459 = DIRECTION ( 'NONE',  ( 0.000000000000000000, 0.000000000000000000, -1.000000000000000000 ) ) ;
#1460 = VERTEX_POINT ( 'NONE', #542 ) ;
#1461 = VERTEX_POINT ( 'NONE', #7436 ) ;
#1462 = DIRECTION ( 'NONE',  ( 0.000000000000000000, 0.000000000000000000, -1.000000000000000000 ) ) ;
#1463 = ORIENTED_EDGE ( 'NONE', *, *, #1965, .T. ) ;
#1464 = APPLICATION_PROTOCOL_DEFINITION ( 'draft international standard', 'automotive_design', 1998, #3711 ) ;
#1465 = EDGE_CURVE ( 'NONE', #10429, #16699, #5929, .T. ) ;
#1466 = CARTESIAN_POINT ( 'NONE',  ( 40.00000000000000711, 136.6227766016838245, 0.000000000000000000 ) ) ;
#1467 = DIRECTION ( 'NONE',  ( 0.000000000000000000, 1.000000000000000000, 0.000000000000000000 ) ) ;
#1468 = CARTESIAN_POINT ( 'NONE',  ( 17.01457324639674695, 29.95810005730942649, -12.72891809691981102 ) ) ;
#1469 = VECTOR ( 'NONE', #5604, 1000.000000000000000 ) ;
#1470 = CARTESIAN_POINT ( 'NONE',  ( -194.2319660531761656, 171.6227766016838245, 0.000000000000000000 ) ) ;
#1471 = CARTESIAN_POINT ( 'NONE',  ( -84.24740733152653149, 149.2783667126899445, 24.28707720053398944 ) ) ;
#1472 = ORIENTED_EDGE ( 'NONE', *, *, #1487, .T. ) ;
#1473 =( BOUNDED_SURFACE ( )  B_SPLINE_SURFACE ( 3, 2, ( 
 ( #15073, #11091, #5618 ),
 ( #212, #9763, #8612 ),
 ( #13759, #380, #4554 ),
 ( #14023, #9853, #7285 ) ),
 .UNSPECIFIED., .F., .F., .F. ) 
 B_SPLINE_SURFACE_WITH_KNOTS ( ( 4, 4 ),
 ( 3, 3 ),
 ( 0.1516087691302827056, 0.1566150273425061523 ),
 ( 0.000000000000000000, 1.000000000000000000 ),
 .UNSPECIFIED. ) 
 GEOMETRIC_REPRESENTATION_ITEM ( )  RATIONAL_B_SPLINE_SURFACE ( (
 ( 1.000000000000000000, 0.6556320892438534109, 1.000000000000000000),
 ( 1.000000000000000000, 0.6556321914870764100, 1.000000000000000000),
 ( 1.000000000000000000, 0.6556957163104859543, 1.000000000000000000),
 ( 1.000000000000000000, 0.6558243695371223092, 1.000000000000000000) ) ) 
 REPRESENTATION_ITEM ( '' )  SURFACE ( )  );
#1474 = CARTESIAN_POINT ( 'NONE',  ( -84.99092202599167933, 199.9711820797445512, -20.53336423377503905 ) ) ;
#1475 = CARTESIAN_POINT ( 'NONE',  ( 17.00000000000000000, 171.6227766016838245, 0.000000000000000000 ) ) ;
#1476 = CARTESIAN_POINT ( 'NONE',  ( 34.26588824652853305, 20.00000000000000355, -10.16858984204336736 ) ) ;
#1477 = FACE_OUTER_BOUND ( 'NONE', #237, .T. ) ;
#1478 = CARTESIAN_POINT ( 'NONE',  ( -33.00000000000000711, 171.6227766016838245, -5.000000000000007994 ) ) ;
#1479 = ORIENTED_EDGE ( 'NONE', *, *, #2590, .F. ) ;
#1480 = CARTESIAN_POINT ( 'NONE',  ( 196.0000000000000000, 163.6227766016838530, 10.00000337241049309 ) ) ;
#1481 = VERTEX_POINT ( 'NONE', #4870 ) ;
#1482 = CARTESIAN_POINT ( 'NONE',  ( -77.50000000000001421, 196.6227766016838245, 10.00000000000000178 ) ) ;
#1483 = ORIENTED_EDGE ( 'NONE', *, *, #845, .F. ) ;
#1484 = EDGE_CURVE ( 'NONE', #3419, #10551, #15402, .T. ) ;
#1485 = EDGE_CURVE ( 'NONE', #17476, #8669, #11468, .T. ) ;
#1486 = CARTESIAN_POINT ( 'NONE',  ( 15.96677753506825681, 136.6227766017765930, -1.239574023933634583 ) ) ;
#1487 = EDGE_CURVE ( 'NONE', #3421, #15746, #11599, .T. ) ;
#1488 = CARTESIAN_POINT ( 'NONE',  ( 49.99999999999998579, 171.6227766016838245, 12.50000337241049131 ) ) ;
#1489 = VERTEX_POINT ( 'NONE', #13999 ) ;
#1490 = CARTESIAN_POINT ( 'NONE',  ( -73.00000000000001421, 171.6227766016838245, 0.000000000000000000 ) ) ;
#1491 = DIRECTION ( 'NONE',  ( 1.000000000000000000, 0.000000000000000000, 0.000000000000000000 ) ) ;
#1492 = FACE_OUTER_BOUND ( 'NONE', #8201, .T. ) ;
#1493 = PLANE ( 'NONE',  #4122 ) ;
#1494 = PRODUCT ( 'Variable Speed Trigger Switch assembly', 'Variable Speed Trigger Switch assembly', '', ( #6686 ) ) ;
#1495 = CARTESIAN_POINT ( 'NONE',  ( 19.90854668962809626, 140.2883655178033848, -15.59737012465792461 ) ) ;
#1496 = ORIENTED_EDGE ( 'NONE', *, *, #10090, .T. ) ;
#1497 = CARTESIAN_POINT ( 'NONE',  ( -27.99999999999998224, 10.00000000000000000, -16.00000000000000000 ) ) ;
#1498 = DIRECTION ( 'NONE',  ( -1.000000000000000000, 0.000000000000000000, 0.000000000000000000 ) ) ;
#1499 = ORIENTED_EDGE ( 'NONE', *, *, #13886, .T. ) ;
#1500 = CARTESIAN_POINT ( 'NONE',  ( -32.59761674097325823, 119.3792650757663978, -5.080178642870992967 ) ) ;
#1501 = CARTESIAN_POINT ( 'NONE',  ( -71.66708739526794147, 110.0000000000000142, -5.500000000000000000 ) ) ;
#1502 = CARTESIAN_POINT ( 'NONE',  ( 27.13113508426156173, 192.5125816722295156, 25.54797519334865896 ) ) ;
#1503 = DIRECTION ( 'NONE',  ( -1.000000000000000000, -6.938893903907228378E-16, -0.000000000000000000 ) ) ;
#1504 = FACE_OUTER_BOUND ( 'NONE', #13698, .T. ) ;
#1505 = DIRECTION ( 'NONE',  ( -0.000000000000000000, -0.000000000000000000, -1.000000000000000000 ) ) ;
#1506 = CARTESIAN_POINT ( 'NONE',  ( -80.00000000000001421, 196.6227766016838245, -13.00000000000000000 ) ) ;
#1507 = CARTESIAN_POINT ( 'NONE',  ( 24.50557348073514063, 144.1870492754457302, -21.73814637783849690 ) ) ;
#1508 = ORIENTED_EDGE ( 'NONE', *, *, #174, .T. ) ;
#1509 = CARTESIAN_POINT ( 'NONE',  ( -17.27091434876127707, 32.11264161353675917, -9.179609695281474302 ) ) ;
#1510 = EDGE_LOOP ( 'NONE', ( #13211, #4341, #7022, #15878, #8880, #5058, #3959, #10219 ) ) ;
#1511 = CARTESIAN_POINT ( 'NONE',  ( 196.0000000000000000, 179.6227766016838245, -12.50000337241049309 ) ) ;
#1512 = CARTESIAN_POINT ( 'NONE',  ( 27.99999999999998224, 9.999999999999998224, 0.000000000000000000 ) ) ;
#1513 = ORIENTED_EDGE ( 'NONE', *, *, #15423, .T. ) ;
#1514 = EDGE_CURVE ( 'NONE', #12210, #16876, #12837, .T. ) ;
#1515 = CARTESIAN_POINT ( 'NONE',  ( -27.84784281930893357, 19.99999999999999645, 7.647248539284095870 ) ) ;
#1516 = CARTESIAN_POINT ( 'NONE',  ( 0.000000000000000000, 18.00000000000000355, -25.00000000000000000 ) ) ;
#1517 = VERTEX_POINT ( 'NONE', #9919 ) ;
#1518 = DIRECTION ( 'NONE',  ( -1.000000000000000000, 0.000000000000000000, 0.000000000000000000 ) ) ;
#1519 = ORIENTED_EDGE ( 'NONE', *, *, #9584, .F. ) ;
#1520 = LINE ( 'NONE', #2601, #13482 ) ;
#1521 = LINE ( 'NONE', #13740, #16390 ) ;
#1522 = CARTESIAN_POINT ( 'NONE',  ( 2.370000000000000551, 5.817072295949927426E-16, -4.750000000000000000 ) ) ;
#1523 = ORIENTED_EDGE ( 'NONE', *, *, #3971, .T. ) ;
#1524 = DIRECTION ( 'NONE',  ( 1.000000000000000000, 0.000000000000000000, 0.000000000000000000 ) ) ;
#1525 = ORIENTED_EDGE ( 'NONE', *, *, #4841, .F. ) ;
#1526 = CARTESIAN_POINT ( 'NONE',  ( -50.00000000000000000, 171.6227766016838245, -20.00000000000000355 ) ) ;
#1527 = ORIENTED_EDGE ( 'NONE', *, *, #15762, .F. ) ;
#1528 = LINE ( 'NONE', #1268, #15237 ) ;
#1529 = CARTESIAN_POINT ( 'NONE',  ( -23.00000000000000000, 122.0000000000000284, 15.00000000000000000 ) ) ;
#1530 = CARTESIAN_POINT ( 'NONE',  ( -9.527527117355448993, 30.70225384978374450, -12.78416694138776855 ) ) ;
#1531 = ORIENTED_EDGE ( 'NONE', *, *, #11203, .F. ) ;
#1532 = ORIENTED_EDGE ( 'NONE', *, *, #5703, .F. ) ;
#1533 = EDGE_CURVE ( 'NONE', #4748, #5251, #15321, .T. ) ;
#1534 = VECTOR ( 'NONE', #15914, 1000.000000000000000 ) ;
#1535 = CIRCLE ( 'NONE', #5210, 2.500000000000002220 ) ;
#1536 = CARTESIAN_POINT ( 'NONE',  ( -72.50000000000000000, 196.6227766016838245, -21.54065922853802562 ) ) ;
#1537 = CARTESIAN_POINT ( 'NONE',  ( 11.58137902169779920, 142.1604892273610687, 18.89461017025931966 ) ) ;
#1538 = EDGE_CURVE ( 'NONE', #3188, #13136, #6102, .T. ) ;
#1539 = ORIENTED_EDGE ( 'NONE', *, *, #14098, .T. ) ;
#1540 = APPLICATION_PROTOCOL_DEFINITION ( 'draft international standard', 'automotive_design', 1998, #4617 ) ;
#1541 = DIRECTION ( 'NONE',  ( 1.000000000000000000, 0.000000000000000000, -0.000000000000000000 ) ) ;
#1542 = ADVANCED_FACE ( 'NONE', ( #1869 ), #4791, .F. ) ;
#1543 = CARTESIAN_POINT ( 'NONE',  ( -73.00000000000001421, 171.6227766016838245, 5.000000000000006217 ) ) ;
#1544 = EDGE_CURVE ( 'NONE', #3796, #17220, #2987, .T. ) ;
#1545 = FACE_OUTER_BOUND ( 'NONE', #435, .T. ) ;
#1546 = FACE_OUTER_BOUND ( 'NONE', #389, .T. ) ;
#1547 = LINE ( 'NONE', #5180, #15428 ) ;
#1548 = AXIS2_PLACEMENT_3D ( 'NONE', #901, #2310, #7701 ) ;
#1549 = ORIENTED_EDGE ( 'NONE', *, *, #279, .F. ) ;
#1550 = DIRECTION ( 'NONE',  ( -0.000000000000000000, -0.000000000000000000, -1.000000000000000000 ) ) ;
#1552 = CARTESIAN_POINT ( 'NONE',  ( 0.000000000000000000, 1.732050807568885631, 0.000000000000000000 ) ) ;
#1551 = AXIS2_PLACEMENT_3D ( 'NONE', #11, #2488, #8234 ) ;
#1553 = FACE_OUTER_BOUND ( 'NONE', #6090, .T. ) ;
#1554 = DIRECTION ( 'NONE',  ( -1.000000000000000000, -0.000000000000000000, -0.000000000000000000 ) ) ;
#1555 = LINE ( 'NONE', #12356, #6673 ) ;
#1556 = ORIENTED_EDGE ( 'NONE', *, *, #1424, .F. ) ;
#1557 = CARTESIAN_POINT ( 'NONE',  ( -68.00000000000000000, 171.6227766016838245, 0.000000000000000000 ) ) ;
#1558 = ORIENTED_EDGE ( 'NONE', *, *, #17219, .F. ) ;
#1559 = LINE ( 'NONE', #6964, #4454 ) ;
#1560 = CIRCLE ( 'NONE', #9186, 6.000000000000008882 ) ;
#1561 = VERTEX_POINT ( 'NONE', #16750 ) ;
#1562 = SURFACE_SIDE_STYLE ('',( #10778 ) ) ;
#1563 = LINE ( 'NONE', #15191, #7080 ) ;
#1564 = COLOUR_RGB ( '', 0.72549020, 0.75294118, 0.79215686) ;
#1565 =( NAMED_UNIT ( * ) SI_UNIT ( $, .STERADIAN. ) SOLID_ANGLE_UNIT ( ) );
#1566 = TOROIDAL_SURFACE ( 'NONE', #3832, 25.00000000000000000, 10.00000000000000000 ) ;
#1567 = CARTESIAN_POINT ( 'NONE',  ( -725.0000000000000000, 19.99999999999995737, 0.000000000000000000 ) ) ;
#1568 = ORIENTED_EDGE ( 'NONE', *, *, #4182, .F. ) ;
#1569 = CARTESIAN_POINT ( 'NONE',  ( -33.00000000000000711, 171.6227766016838245, 0.000000000000000000 ) ) ;
#1570 = DIRECTION ( 'NONE',  ( 0.000000000000000000, 0.000000000000000000, 1.000000000000000000 ) ) ;
#1571 = FACE_OUTER_BOUND ( 'NONE', #7575, .T. ) ;
#1572 = CARTESIAN_POINT ( 'NONE',  ( 49.99999999999998579, 155.6227766016839098, -15.00000337241049486 ) ) ;
#1573 = PRESENTATION_LAYER_ASSIGNMENT (  '', '', ( #1297 ) ) ;
#1574 = EDGE_CURVE ( 'NONE', #14903, #9038, #2433, .T. ) ;
#1575 = ADVANCED_FACE ( 'NONE', ( #8848 ), #117, .T. ) ;
#1576 = AXIS2_PLACEMENT_3D ( 'NONE', #14573, #2356, #8015 ) ;
#1577 = VECTOR ( 'NONE', #9354, 1000.000000000000000 ) ;
#1578 = AXIS2_PLACEMENT_3D ( 'NONE', #57, #11911, #5457 ) ;
#1579 = CARTESIAN_POINT ( 'NONE',  ( 16.78995144247101123, 126.8031893778130410, -8.318227863269529010 ) ) ;
#1580 = ORIENTED_EDGE ( 'NONE', *, *, #10878, .T. ) ;
#1581 = FACE_OUTER_BOUND ( 'NONE', #1905, .T. ) ;
#1582 = CARTESIAN_POINT ( 'NONE',  ( 13.63270490666636192, 138.8028880870465969, -3.449993069226350517 ) ) ;
#1583 = VERTEX_POINT ( 'NONE', #10868 ) ;
#1584 = CARTESIAN_POINT ( 'NONE',  ( -79.76522515338450603, 190.6230697630495001, -29.39368741583861677 ) ) ;
#1585 = CLOSED_SHELL ( 'NONE', ( #12508, #15158, #17233, #3535, #8065, #16357, #12591, #1655, #12803, #4422, #689, #10482, #7807, #15850, #9522, #5248, #16253, #9807 ) ) ;
#1586 = VECTOR ( 'NONE', #4728, 1000.000000000000000 ) ;
#1587 = CARTESIAN_POINT ( 'NONE',  ( -22.99999999999999645, 90.00000000000000000, 0.000000000000000000 ) ) ;
#1588 = CIRCLE ( 'NONE', #16861, 1.500000000000000000 ) ;
#1589 = CYLINDRICAL_SURFACE ( 'NONE', #12637, 9.999999999999994671 ) ;
#1590 = DIRECTION ( 'NONE',  ( -0.000000000000000000, 0.000000000000000000, -1.000000000000000000 ) ) ;
#1591 = DIRECTION ( 'NONE',  ( -5.638339401448894059E-16, -0.000000000000000000, -1.000000000000000000 ) ) ;
#1592 = CARTESIAN_POINT ( 'NONE',  ( 21.29916379186985154, 29.87370047437059384, 9.875089623381150261 ) ) ;
#1593 = CARTESIAN_POINT ( 'NONE',  ( -45.00000000000000000, 134.2062027339443944, 25.00000000000000000 ) ) ;
#1594 = FACE_BOUND ( 'NONE', #9557, .T. ) ;
#1595 = EDGE_LOOP ( 'NONE', ( #13949, #10949, #5695, #10028 ) ) ;
#1596 = CARTESIAN_POINT ( 'NONE',  ( -19.26597175465490963, 19.99999999999999645, -21.35691006828317384 ) ) ;
#1597 = EDGE_CURVE ( 'NONE', #1517, #16267, #2739, .T. ) ;
#1598 = EDGE_CURVE ( 'NONE', #5268, #5255, #15155, .T. ) ;
#1599 = EDGE_CURVE ( 'NONE', #2257, #15641, #8923, .T. ) ;
#1600 = EDGE_LOOP ( 'NONE', ( #2861, #12870, #15823, #5940 ) ) ;
#1601 = EDGE_CURVE ( 'NONE', #647, #15581, #1677, .T. ) ;
#1602 = VECTOR ( 'NONE', #10888, 1000.000000000000000 ) ;
#1603 = CIRCLE ( 'NONE', #9796, 20.00000000000000355 ) ;
#1604 = CARTESIAN_POINT ( 'NONE',  ( 22.93524650466160963, 29.84210526315773748, -15.00000000000000000 ) ) ;
#1605 = VECTOR ( 'NONE', #16210, 1000.000000000000000 ) ;
#1606 = ORIENTED_EDGE ( 'NONE', *, *, #13785, .T. ) ;
#1607 = FACE_OUTER_BOUND ( 'NONE', #1211, .T. ) ;
#1608 = AXIS2_PLACEMENT_3D ( 'NONE', #16914, #3374, #714 ) ;
#1609 = LINE ( 'NONE', #7008, #15259 ) ;
#1610 = ORIENTED_EDGE ( 'NONE', *, *, #13821, .F. ) ;
#1611 = CARTESIAN_POINT ( 'NONE',  ( 30.30638721710497663, 154.1221233254128151, -27.97726104294732608 ) ) ;
#1612 = CARTESIAN_POINT ( 'NONE',  ( -21.99999999999998579, 10.00000000000000000, -35.00000000000000000 ) ) ;
#1613 = FACE_OUTER_BOUND ( 'NONE', #14014, .T. ) ;
#1614 = AXIS2_PLACEMENT_3D ( 'NONE', #4696, #8584, #7260 ) ;
#1615 = CARTESIAN_POINT ( 'NONE',  ( 37.34664361473878103, 195.0609035571773404, -23.23759988234784046 ) ) ;
#1616 = DIRECTION ( 'NONE',  ( -0.9940220915700700433, 0.1091791256177803010, 0.000000000000000000 ) ) ;
#1617 = AXIS2_PLACEMENT_3D ( 'NONE', #9296, #13195, #13373 ) ;
#1618 = FACE_OUTER_BOUND ( 'NONE', #10580, .T. ) ;
#1619 = EDGE_CURVE ( 'NONE', #10750, #7725, #11750, .T. ) ;
#1620 = STYLED_ITEM ( 'NONE', ( #7941 ), #16900 ) ;
#1621 = DIRECTION ( 'NONE',  ( -1.000000000000000000, 0.000000000000000000, 0.000000000000000000 ) ) ;
#1622 = ORIENTED_EDGE ( 'NONE', *, *, #11806, .T. ) ;
#1623 = CARTESIAN_POINT ( 'NONE',  ( 49.99999999999998579, 151.6227766016839098, 5.571800142134973655 ) ) ;
#1624 = ORIENTED_EDGE ( 'NONE', *, *, #15388, .T. ) ;
#1625 = PLANE ( 'NONE',  #5932 ) ;
#1626 = LINE ( 'NONE', #12244, #17139 ) ;
#1627 = ORIENTED_EDGE ( 'NONE', *, *, #7314, .F. ) ;
#1628 = EDGE_LOOP ( 'NONE', ( #8218, #8255, #7962, #5508 ) ) ;
#1629 = EDGE_LOOP ( 'NONE', ( #3743, #16683, #6844, #9775 ) ) ;
#1630 = CARTESIAN_POINT ( 'NONE',  ( -100.0000000000000000, 136.6227766016838245, 0.000000000000000000 ) ) ;
#1631 = VECTOR ( 'NONE', #13356, 1000.000000000000000 ) ;
#1632 = CARTESIAN_POINT ( 'NONE',  ( -48.00000000000000000, 171.6227766016838245, 20.00000000000000355 ) ) ;
#1634 = CARTESIAN_POINT ( 'NONE',  ( 13.88882648224844907, 138.0291231684843751, 11.40862608215693008 ) ) ;
#1633 = PRODUCT_DEFINITION_FORMATION_WITH_SPECIFIED_SOURCE ( 'ANY', '', #8716, .NOT_KNOWN. ) ;
#1635 = AXIS2_PLACEMENT_3D ( 'NONE', #14995, #2869, #1277 ) ;
#1636 = ORIENTED_EDGE ( 'NONE', *, *, #12412, .T. ) ;
#1637 = CARTESIAN_POINT ( 'NONE',  ( 27.50000000000001066, 146.6227766016838245, 1.387778780781445676E-14 ) ) ;
#1638 = CARTESIAN_POINT ( 'NONE',  ( 40.00000000000000711, 171.6227766016838245, 0.000000000000000000 ) ) ;
#1639 = CARTESIAN_POINT ( 'NONE',  ( 15.46067906867578046, 29.98929614515185804, -13.00000000000000533 ) ) ;
#1640 = CARTESIAN_POINT ( 'NONE',  ( 49.99999999999998579, 167.6227766016838530, -5.571800142134975431 ) ) ;
#1641 = FACE_OUTER_BOUND ( 'NONE', #10671, .T. ) ;
#1642 = EDGE_CURVE ( 'NONE', #4930, #5440, #7783, .T. ) ;
#1643 = ORIENTED_EDGE ( 'NONE', *, *, #16262, .F. ) ;
#1644 = CARTESIAN_POINT ( 'NONE',  ( -32.02886766642248517, 100.0581520846466930, 5.500000000000000000 ) ) ;
#1645 = AXIS2_PLACEMENT_3D ( 'NONE', #1452, #13317, #1181 ) ;
#1646 = CARTESIAN_POINT ( 'NONE',  ( 34.93420767853316988, 30.00000000000000000, 0.000000000000000000 ) ) ;
#1647 = CARTESIAN_POINT ( 'NONE',  ( 16.25302816831168329, 19.99999999999999645, -25.00000000000000000 ) ) ;
#1648 = CARTESIAN_POINT ( 'NONE',  ( -206.8260782938592968, 173.5737298318736350, 4.615523682683083884 ) ) ;
#1649 = CIRCLE ( 'NONE', #10973, 2.500000000000002220 ) ;
#1650 = CARTESIAN_POINT ( 'NONE',  ( 32.50000000000000000, 196.6227766016838245, 10.00000000000000178 ) ) ;
#1651 = PRODUCT_DEFINITION_CONTEXT ( 'detailed design', #14329, 'design' ) ;
#1652 = VERTEX_POINT ( 'NONE', #12212 ) ;
#1653 = EDGE_CURVE ( 'NONE', #13207, #13081, #82, .T. ) ;
#1654 = VERTEX_POINT ( 'NONE', #16205 ) ;
#1655 = ADVANCED_FACE ( 'NONE', ( #13541 ), #14946, .T. ) ;
#1656 = EDGE_CURVE ( 'NONE', #7107, #399, #16284, .T. ) ;
#1657 = DIRECTION ( 'NONE',  ( 1.000000000000000000, 0.000000000000000000, 0.000000000000000000 ) ) ;
#1658 = EDGE_LOOP ( 'NONE', ( #1744, #8467, #2560, #5454, #5419, #7001 ) ) ;
#1659 = CARTESIAN_POINT ( 'NONE',  ( -45.00000000000000000, 130.0000000000000000, 0.000000000000000000 ) ) ;
#1660 = ORIENTED_EDGE ( 'NONE', *, *, #7972, .T. ) ;
#1661 = CARTESIAN_POINT ( 'NONE',  ( 17.54349574104652021, 125.4948194589026684, -5.000000000000000888 ) ) ;
#1662 = VECTOR ( 'NONE', #12747, 1000.000000000000000 ) ;
#1663 = SURFACE_STYLE_USAGE ( .BOTH. , #5645 ) ;
#1664 = CARTESIAN_POINT ( 'NONE',  ( -208.1243352336975079, 166.1145920781434029, 2.051787360128269899 ) ) ;
#1665 = FACE_OUTER_BOUND ( 'NONE', #17509, .T. ) ;
#1666 = EDGE_LOOP ( 'NONE', ( #926, #20 ) ) ;
#1667 = DIRECTION ( 'NONE',  ( -1.000000000000000000, 0.000000000000000000, 0.000000000000000000 ) ) ;
#1668 = PLANE ( 'NONE',  #16897 ) ;
#1669 = FACE_OUTER_BOUND ( 'NONE', #6501, .T. ) ;
#1670 = AXIS2_PLACEMENT_3D ( 'NONE', #11861, #14612, #14871 ) ;
#1671 = AXIS2_PLACEMENT_3D ( 'NONE', #11024, #4308, #9688 ) ;
#1672 = AXIS2_PLACEMENT_3D ( 'NONE', #15684, #2507, #11883 ) ;
#1673 = ADVANCED_FACE ( 'NONE', ( #162 ), #12026, .F. ) ;
#1674 = CARTESIAN_POINT ( 'NONE',  ( 27.42233524417435930, 136.9585154912620908, -4.953423069178740867 ) ) ;
#1675 = ORIENTED_EDGE ( 'NONE', *, *, #5899, .T. ) ;
#1676 = CARTESIAN_POINT ( 'NONE',  ( -74.00000000000005684, 147.2627523208502112, -25.14806991105193035 ) ) ;
#1677 = LINE ( 'NONE', #5658, #4973 ) ;
#1678 = ORIENTED_EDGE ( 'NONE', *, *, #13570, .T. ) ;
#1679 = CARTESIAN_POINT ( 'NONE',  ( -81.78007429493302993, 190.8885537947572857, -29.22050223063088836 ) ) ;
#1680 = CARTESIAN_POINT ( 'NONE',  ( -80.00000000000002842, 146.6227766016838245, -35.00200000000000244 ) ) ;
#1681 = AXIS2_PLACEMENT_3D ( 'NONE', #8742, #863, #6079 ) ;
#1682 = EDGE_CURVE ( 'NONE', #14446, #5655, #10962, .T. ) ;
#1683 = CIRCLE ( 'NONE', #13723, 6.000000000000008882 ) ;
#1684 = DIRECTION ( 'NONE',  ( -1.000000000000000000, 0.000000000000000000, 0.000000000000000000 ) ) ;
#1685 = AXIS2_PLACEMENT_3D ( 'NONE', #2929, #1783, #1518 ) ;
#1686 = CARTESIAN_POINT ( 'NONE',  ( -80.00000000000001421, 196.6227766016838245, 0.000000000000000000 ) ) ;
#1687 = FACE_OUTER_BOUND ( 'NONE', #6399, .T. ) ;
#1688 = CARTESIAN_POINT ( 'NONE',  ( -100.0000000000000000, 143.9321776784423150, 5.086680500673126297E-15 ) ) ;
#1689 = CARTESIAN_POINT ( 'NONE',  ( -81.15920507698956499, 201.4909985710883404, 14.03234625026782645 ) ) ;
#1690 = DIRECTION ( 'NONE',  ( 0.000000000000000000, 0.000000000000000000, 1.000000000000000000 ) ) ;
#1691 = ORIENTED_EDGE ( 'NONE', *, *, #15361, .T. ) ;
#1692 = ORIENTED_EDGE ( 'NONE', *, *, #9652, .F. ) ;
#1693 = DIRECTION ( 'NONE',  ( -0.000000000000000000, -0.000000000000000000, 1.000000000000000000 ) ) ;
#1694 = VECTOR ( 'NONE', #11931, 1000.000000000000000 ) ;
#1695 = PLANE ( 'NONE',  #2738 ) ;
#1696 = VERTEX_POINT ( 'NONE', #8098 ) ;
#1697 = CARTESIAN_POINT ( 'NONE',  ( -14.66060021943786751, 20.00000000000115818, 8.782938007015319570 ) ) ;
#1698 = VECTOR ( 'NONE', #6202, 1000.000000000000000 ) ;
#1699 = DIRECTION ( 'NONE',  ( 0.000000000000000000, 0.000000000000000000, -1.000000000000000000 ) ) ;
#1700 = EDGE_LOOP ( 'NONE', ( #10050, #15247, #3822 ) ) ;
#1701 = CARTESIAN_POINT ( 'NONE',  ( 37.50000000000001421, 197.1883573205068103, -20.88424858573644372 ) ) ;
#1702 = CARTESIAN_POINT ( 'NONE',  ( -10.03891356649073785, 18.00000000000000355, 24.87483525495233394 ) ) ;
#1703 = EDGE_CURVE ( 'NONE', #15972, #8380, #13516, .T. ) ;
#1704 = EDGE_CURVE ( 'NONE', #11501, #11034, #7847, .T. ) ;
#1705 = EDGE_CURVE ( 'NONE', #12616, #16016, #6950, .T. ) ;
#1706 = CARTESIAN_POINT ( 'NONE',  ( -207.9324504923922916, 166.2413418076914979, -1.515671747849433926 ) ) ;
#1707 = PLANE ( 'NONE',  #14282 ) ;
#1708 = CIRCLE ( 'NONE', #4246, 5.000000000000018652 ) ;
#1709 = DIRECTION ( 'NONE',  ( -1.156482317317868274E-16, 1.000000000000000000, 0.000000000000000000 ) ) ;
#1710 = CARTESIAN_POINT ( 'NONE',  ( -22.99999999999998224, 10.00000000000000000, -12.99999999999999822 ) ) ;
#1711 = CIRCLE ( 'NONE', #3418, 2.500000000000002220 ) ;
#1712 = CARTESIAN_POINT ( 'NONE',  ( -3.000000000000000888, 154.3022685259950038, -9.999999999999900524 ) ) ;
#1713 = ORIENTED_EDGE ( 'NONE', *, *, #15281, .T. ) ;
#1714 = CARTESIAN_POINT ( 'NONE',  ( -151.0000000000000284, 171.6227766016838245, 0.000000000000000000 ) ) ;
#1715 = ORIENTED_EDGE ( 'NONE', *, *, #6823, .F. ) ;
#1716 = FACE_OUTER_BOUND ( 'NONE', #8856, .T. ) ;
#1717 = CARTESIAN_POINT ( 'NONE',  ( -11.09520285051611488, 31.19962993084977398, -12.30130330100619673 ) ) ;
#1718 = VERTEX_POINT ( 'NONE', #17503 ) ;
#1719 = EDGE_LOOP ( 'NONE', ( #15688, #11199 ) ) ;
#1720 = CARTESIAN_POINT ( 'NONE',  ( 34.93420767853316988, 18.00000000000000355, 0.000000000000000000 ) ) ;
#1721 = ADVANCED_BREP_SHAPE_REPRESENTATION ( '', ( #11363, #3583 ), #3025 ) ;
#1722 = AXIS2_PLACEMENT_3D ( 'NONE', #2794, #16251, #2704 ) ;
#1723 = LINE ( 'NONE', #1632, #8183 ) ;
#1724 = CARTESIAN_POINT ( 'NONE',  ( 16.97810798871989135, 126.5456571586929044, 7.842726245482330327 ) ) ;
#1725 = ORIENTED_EDGE ( 'NONE', *, *, #15661, .T. ) ;
#1726 = CARTESIAN_POINT ( 'NONE',  ( 196.0000000000000000, 179.6227766016838245, -12.50000337241049309 ) ) ;
#1727 = EDGE_CURVE ( 'NONE', #1279, #14060, #14855, .T. ) ;
#1728 = CARTESIAN_POINT ( 'NONE',  ( -33.00000000000000711, 171.6227766016838245, 0.000000000000000000 ) ) ;
#1729 = DIRECTION ( 'NONE',  ( 0.000000000000000000, 0.000000000000000000, 1.000000000000000000 ) ) ;
#1730 = CARTESIAN_POINT ( 'NONE',  ( 18.93266870823487125, 29.92002005853035840, 11.93384102663519997 ) ) ;
#1731 = CARTESIAN_POINT ( 'NONE',  ( 0.000000000000000000, 0.8660254037844428154, 1.500000000000001332 ) ) ;
#1732 = ORIENTED_EDGE ( 'NONE', *, *, #12889, .T. ) ;
#1733 = CARTESIAN_POINT ( 'NONE',  ( 27.48361012698976324, 138.6227766016838245, -1.226160068396871639 ) ) ;
#1734 = CIRCLE ( 'NONE', #6249, 2.499999999999998668 ) ;
#1735 = CARTESIAN_POINT ( 'NONE',  ( 1.559999999999998943, -1.732050807568885631, 0.000000000000000000 ) ) ;
#1736 = DIRECTION ( 'NONE',  ( 0.000000000000000000, -1.000000000000000000, 0.000000000000000000 ) ) ;
#1737 = FACE_OUTER_BOUND ( 'NONE', #5723, .T. ) ;
#1738 = CARTESIAN_POINT ( 'NONE',  ( 37.99999999999998579, 20.00000000000000000, 28.00000000000001066 ) ) ;
#1739 = ORIENTED_EDGE ( 'NONE', *, *, #2762, .T. ) ;
#1740 = ORIENTED_EDGE ( 'NONE', *, *, #6843, .T. ) ;
#1741 = LINE ( 'NONE', #5801, #6222 ) ;
#1742 = ORIENTED_EDGE ( 'NONE', *, *, #3445, .F. ) ;
#1743 = ADVANCED_FACE ( 'NONE', ( #5373 ), #6520, .F. ) ;
#1744 = ORIENTED_EDGE ( 'NONE', *, *, #1140, .F. ) ;
#1745 = APPLICATION_PROTOCOL_DEFINITION ( 'draft international standard', 'automotive_design', 1998, #86 ) ;
#1746 = DIRECTION ( 'NONE',  ( 1.000000000000000000, 0.000000000000000000, 0.000000000000000000 ) ) ;
#1747 =( NAMED_UNIT ( * ) PLANE_ANGLE_UNIT ( ) SI_UNIT ( $, .RADIAN. ) );
#1748 = CARTESIAN_POINT ( 'NONE',  ( -207.9328752093750836, 166.2410986792852725, 1.516464574996131409 ) ) ;
#1749 = DIRECTION ( 'NONE',  ( -1.000000000000000000, 0.000000000000000000, 0.000000000000000000 ) ) ;
#1750 = CARTESIAN_POINT ( 'NONE',  ( 22.42543865150203075, 29.85191494357712116, -7.821916630904659939 ) ) ;
#1751 = ORIENTED_EDGE ( 'NONE', *, *, #5331, .T. ) ;
#1752 = CARTESIAN_POINT ( 'NONE',  ( 31.13043979496999114, 141.7478424248371596, 14.01801864773823070 ) ) ;
#1753 = DIRECTION ( 'NONE',  ( -0.000000000000000000, -0.000000000000000000, -1.000000000000000000 ) ) ;
#1754 = DIRECTION ( 'NONE',  ( -1.156482317317868274E-16, 1.000000000000000000, 0.000000000000000000 ) ) ;
#1755 = DIRECTION ( 'NONE',  ( 0.000000000000000000, 0.000000000000000000, -1.000000000000000000 ) ) ;
#1756 = DIRECTION ( 'NONE',  ( 1.000000000000000000, 0.000000000000000000, 0.000000000000000000 ) ) ;
#1757 = VERTEX_POINT ( 'NONE', #13153 ) ;
#1758 = EDGE_CURVE ( 'NONE', #3754, #2297, #9190, .T. ) ;
#1759 = CARTESIAN_POINT ( 'NONE',  ( 30.00000000000001066, 146.6227766016838245, -35.00200000000000244 ) ) ;
#1760 = ORIENTED_EDGE ( 'NONE', *, *, #1075, .F. ) ;
#1761 = FILL_AREA_STYLE ('',( #3087 ) ) ;
#1762 = CARTESIAN_POINT ( 'NONE',  ( -82.20184637777194325, 191.0369151440704343, -29.12214185324409499 ) ) ;
#1763 = DIRECTION ( 'NONE',  ( -0.000000000000000000, -0.000000000000000000, -1.000000000000000000 ) ) ;
#1764 = ADVANCED_FACE ( 'NONE', ( #14755 ), #1566, .T. ) ;
#1765 = CARTESIAN_POINT ( 'NONE',  ( 32.57588347945782914, 192.3210352480456891, 25.70268529851925265 ) ) ;
#1766 = EDGE_CURVE ( 'NONE', #8027, #5289, #14022, .T. ) ;
#1767 = DIRECTION ( 'NONE',  ( 0.000000000000000000, 0.000000000000000000, -1.000000000000000000 ) ) ;
#1768 = ADVANCED_FACE ( 'NONE', ( #5103 ), #17404, .F. ) ;
#1769 = CARTESIAN_POINT ( 'NONE',  ( 27.50000000000000355, 196.6227766016838245, -16.00000000000000000 ) ) ;
#1770 = DIRECTION ( 'NONE',  ( -1.000000000000000000, -0.000000000000000000, 0.000000000000000000 ) ) ;
#1771 = CARTESIAN_POINT ( 'NONE',  ( -83.64566403027420449, 200.0568792608332558, 16.75365501014451297 ) ) ;
#1772 = FACE_BOUND ( 'NONE', #15279, .T. ) ;
#1773 = VERTEX_POINT ( 'NONE', #1203 ) ;
#1774 = ORIENTED_EDGE ( 'NONE', *, *, #8939, .F. ) ;
#1775 = CARTESIAN_POINT ( 'NONE',  ( -96.00000000000001421, 201.6227766016838245, 0.000000000000000000 ) ) ;
#1776 = CARTESIAN_POINT ( 'NONE',  ( 30.00000000000000355, 196.6227766016838245, -13.00000000000000000 ) ) ;
#1777 = ADVANCED_FACE ( 'NONE', ( #12000 ), #5275, .T. ) ;
#1778 = ORIENTED_EDGE ( 'NONE', *, *, #14248, .T. ) ;
#1779 = CARTESIAN_POINT ( 'NONE',  ( -25.81900932159183526, 19.99999999999999645, 13.95463872937544991 ) ) ;
#1780 = CARTESIAN_POINT ( 'NONE',  ( 2.749999999999999112, 0.000000000000000000, 0.000000000000000000 ) ) ;
#1781 = ORIENTED_EDGE ( 'NONE', *, *, #10186, .F. ) ;
#1782 = PRODUCT ( 'Left Housing Shell', 'Left Housing Shell', '', ( #15076 ) ) ;
#1783 = DIRECTION ( 'NONE',  ( -0.000000000000000000, -0.000000000000000000, -1.000000000000000000 ) ) ;
#1784 = LINE ( 'NONE', #1612, #17271 ) ;
#1785 = CARTESIAN_POINT ( 'NONE',  ( 27.99999999999998224, 9.999999999999998224, -16.00000000000000000 ) ) ;
#1786 = CARTESIAN_POINT ( 'NONE',  ( -14.99999999999998579, 90.00000000000000000, -4.999999999999999112 ) ) ;
#1787 = CARTESIAN_POINT ( 'NONE',  ( -24.99999999999999645, 120.0000000000000284, 15.00000000000000000 ) ) ;
#1788 = DIRECTION ( 'NONE',  ( -1.000000000000000000, 0.000000000000000000, 0.000000000000000000 ) ) ;
#1789 = CARTESIAN_POINT ( 'NONE',  ( -68.00000000000000000, 171.6227766016838245, -25.00000000000000000 ) ) ;
#1790 = ORIENTED_EDGE ( 'NONE', *, *, #15077, .T. ) ;
#1791 = CARTESIAN_POINT ( 'NONE',  ( 20.99355996702781724, 139.9415946336124534, -14.89340340269096785 ) ) ;
#1792 = EDGE_LOOP ( 'NONE', ( #8992, #15963, #14025, #11089 ) ) ;
#1793 = CARTESIAN_POINT ( 'NONE',  ( -72.53671098836048259, 195.8564978660713791, -22.40111672564487222 ) ) ;
#1794 = EDGE_CURVE ( 'NONE', #8971, #9872, #3149, .T. ) ;
#1795 = CARTESIAN_POINT ( 'NONE',  ( -13.87134331504352325, 32.05147385205248867, -10.53504704850738705 ) ) ;
#1796 = EDGE_CURVE ( 'NONE', #4487, #8664, #5540, .T. ) ;
#1797 = ORIENTED_EDGE ( 'NONE', *, *, #12196, .F. ) ;
#1798 = ADVANCED_FACE ( 'NONE', ( #12354 ), #7047, .F. ) ;
#1799 = VERTEX_POINT ( 'NONE', #11023 ) ;
#1800 = DIRECTION ( 'NONE',  ( 0.000000000000000000, 0.000000000000000000, -1.000000000000000000 ) ) ;
#1801 = CARTESIAN_POINT ( 'NONE',  ( 1.559999999999998943, 0.8660254037844428154, -1.499999999999997780 ) ) ;
#1802 = CARTESIAN_POINT ( 'NONE',  ( 14.43747245749253416, 129.4010981426196736, 11.63709869316310908 ) ) ;
#1803 = VERTEX_POINT ( 'NONE', #3052 ) ;
#1804 = PLANE ( 'NONE',  #16988 ) ;
#1805 = DIRECTION ( 'NONE',  ( 0.000000000000000000, 0.000000000000000000, 1.000000000000000000 ) ) ;
#1806 = FACE_OUTER_BOUND ( 'NONE', #8014, .T. ) ;
#1807 = DIRECTION ( 'NONE',  ( -0.000000000000000000, -0.000000000000000000, -1.000000000000000000 ) ) ;
#1808 = CARTESIAN_POINT ( 'NONE',  ( 18.47042353409679194, 29.92915261368834479, 12.18054208566702279 ) ) ;
#1809 = DIRECTION ( 'NONE',  ( -1.000000000000000000, 0.000000000000000000, 0.000000000000000000 ) ) ;
#1810 = EDGE_LOOP ( 'NONE', ( #10775, #17313, #13497, #14550 ) ) ;
#1811 = DIRECTION ( 'NONE',  ( 0.000000000000000000, 0.4999999999999996669, 0.8660254037844388186 ) ) ;
#1812 = DIRECTION ( 'NONE',  ( 0.000000000000000000, 0.000000000000000000, 1.000000000000000000 ) ) ;
#1813 = CARTESIAN_POINT ( 'NONE',  ( 29.54149365486396661, 20.00000000000000711, -18.67620474358521676 ) ) ;
#1814 = PLANE ( 'NONE',  #9010 ) ;
#1815 = CARTESIAN_POINT ( 'NONE',  ( -25.00000000000002132, 100.0000000000000142, -4.999999999999999112 ) ) ;
#1816 = AXIS2_PLACEMENT_3D ( 'NONE', #4935, #14324, #11582 ) ;
#1817 = ADVANCED_FACE ( 'NONE', ( #1553 ), #12613, .F. ) ;
#1818 = ORIENTED_EDGE ( 'NONE', *, *, #3538, .T. ) ;
#1819 = EDGE_CURVE ( 'NONE', #2616, #2637, #12891, .T. ) ;
#1820 = VERTEX_POINT ( 'NONE', #2883 ) ;
#1821 = ORIENTED_EDGE ( 'NONE', *, *, #14197, .T. ) ;
#1822 = CARTESIAN_POINT ( 'NONE',  ( 6.134011831684059501, 134.2062027339443944, 13.00000000000000000 ) ) ;
#1823 = EDGE_LOOP ( 'NONE', ( #3154, #257, #5205, #13680 ) ) ;
#1824 = ORIENTED_EDGE ( 'NONE', *, *, #17265, .F. ) ;
#1825 =( LENGTH_UNIT ( ) NAMED_UNIT ( * ) SI_UNIT ( .MILLI., .METRE. ) );
#1826 = CARTESIAN_POINT ( 'NONE',  ( 22.56315672547017925, 145.5208630140649859, -20.20962120078073454 ) ) ;
#1827 = AXIS2_PLACEMENT_3D ( 'NONE', #10901, #9486, #1359 ) ;
#1828 = CARTESIAN_POINT ( 'NONE',  ( 0.000000000000000000, 20.00000000000000000, 0.000000000000000000 ) ) ;
#1829 = CARTESIAN_POINT ( 'NONE',  ( 36.65363293176816484, 143.1278587772777087, -16.66575456205189454 ) ) ;
#1830 = MECHANICAL_DESIGN_GEOMETRIC_PRESENTATION_REPRESENTATION (  '', ( #15396 ), #8611 ) ;
#1831 = EDGE_LOOP ( 'NONE', ( #6276, #7051, #12, #6157 ) ) ;
#1832 = CARTESIAN_POINT ( 'NONE',  ( 0.000000000000000000, 0.000000000000000000, 0.000000000000000000 ) ) ;
#1833 = PLANE ( 'NONE',  #14966 ) ;
#1834 = DIRECTION ( 'NONE',  ( -0.000000000000000000, -0.000000000000000000, 1.000000000000000000 ) ) ;
#1835 = ADVANCED_FACE ( 'NONE', ( #4126 ), #5632, .F. ) ;
#1836 = PRESENTATION_STYLE_ASSIGNMENT (( #11217 ) ) ;
#1837 = CIRCLE ( 'NONE', #14558, 2.499999999999998668 ) ;
#1838 = DIRECTION ( 'NONE',  ( 1.000000000000000000, 0.000000000000000000, 0.000000000000000000 ) ) ;
#1839 = CIRCLE ( 'NONE', #4672, 7.500000000000007105 ) ;
#1840 = ORIENTED_EDGE ( 'NONE', *, *, #2784, .F. ) ;
#1841 = CARTESIAN_POINT ( 'NONE',  ( 14.93242934743711992, 20.00000000000000000, 25.00000000000000000 ) ) ;
#1842 = EDGE_LOOP ( 'NONE', ( #6707, #13226, #11700, #4645 ) ) ;
#1843 = PRESENTATION_STYLE_ASSIGNMENT (( #8568 ) ) ;
#1844 = B_SPLINE_CURVE_WITH_KNOTS ( 'NONE', 3,
 ( #8174, #11087, #2865, #16587 ),
 .UNSPECIFIED., .F., .F.,
 ( 4, 4 ),
 ( 0.001580575003428885293, 0.001893147295999754844 ),
 .UNSPECIFIED. ) ;
#1845 = LINE ( 'NONE', #12745, #6506 ) ;
#1846 = ORIENTED_EDGE ( 'NONE', *, *, #1094, .T. ) ;
#1847 = CARTESIAN_POINT ( 'NONE',  ( 48.00000000000000711, 179.6227766016838245, 10.00000337241049309 ) ) ;
#1848 = CARTESIAN_POINT ( 'NONE',  ( 21.44211297938456084, 29.87092986353274426, 9.660732976998257726 ) ) ;
#1849 = CARTESIAN_POINT ( 'NONE',  ( -31.66708739526795924, 119.0000000000000284, 5.500000000000000000 ) ) ;
#1850 = ORIENTED_EDGE ( 'NONE', *, *, #14310, .F. ) ;
#1851 = CARTESIAN_POINT ( 'NONE',  ( -100.0000000000000000, 142.5209969267753820, -19.44444444444445352 ) ) ;
#1852 = CARTESIAN_POINT ( 'NONE',  ( 15.98317902225257470, 29.97876603371781457, 12.94822346880645902 ) ) ;
#1853 = AXIS2_PLACEMENT_3D ( 'NONE', #13518, #6796, #12191 ) ;
#1854 = CARTESIAN_POINT ( 'NONE',  ( -78.29008794608814981, 201.3251192758334582, 14.38044245167806423 ) ) ;
#1855 = EDGE_CURVE ( 'NONE', #11143, #17364, #4482, .T. ) ;
#1856 = CIRCLE ( 'NONE', #11734, 2.499999999999998668 ) ;
#1857 = CARTESIAN_POINT ( 'NONE',  ( 39.99999999999998579, 4.000000000000007994, 33.00000000000001421 ) ) ;
#1858 = ORIENTED_EDGE ( 'NONE', *, *, #13622, .T. ) ;
#1859 = EDGE_CURVE ( 'NONE', #15841, #6861, #3373, .T. ) ;
#1860 = ORIENTED_EDGE ( 'NONE', *, *, #2897, .F. ) ;
#1861 = CARTESIAN_POINT ( 'NONE',  ( 23.61360151038711308, 29.88540148010350705, -10.01045486545366181 ) ) ;
#1862 = EDGE_CURVE ( 'NONE', #6587, #8018, #8542, .T. ) ;
#1863 = DIRECTION ( 'NONE',  ( 0.000000000000000000, 0.000000000000000000, 1.000000000000000000 ) ) ;
#1864 = EDGE_LOOP ( 'NONE', ( #10980, #15166, #1947, #7705 ) ) ;
#1865 = EDGE_CURVE ( 'NONE', #5946, #12617, #3846, .T. ) ;
#1866 = DIRECTION ( 'NONE',  ( 1.000000000000000000, -0.000000000000000000, -0.000000000000000000 ) ) ;
#1867 = ADVANCED_FACE ( 'NONE', ( #5019, #10412 ), #123, .T. ) ;
#1868 = CLOSED_SHELL ( 'NONE', ( #6036, #7114, #11055, #5318, #17494, #5701, #5862, #391, #9641, #2040, #1798, #8408, #12670, #15046, #6749, #6790, #6995, #3837, #14323, #10466, #12178, #17096, #6391, #16760, #7971, #15007, #16774, #3602, #13406, #7593, #2605, #17289, #16476, #16402, #3138, #8922, #8192, #13603, #6578, #11483, #14202, #76, #3297, #15872, #10123, #5597, #13427, #4544, #10743, #540, #11103, #14161, #9647, #7625, #6284, #8136, #8266, #6925, #2131, #1542, #15587, #14762, #12845, #9828, #14511, #16386, #8426, #17332, #9333, #10127, #16315, #2168, #4742, #1191, #15446, #12099, #688, #1835, #4084, #11756, #5647, #15658, #16639, #14788, #15761, #14281, #8463, #5666, #14905, #12248, #7646, #13752, #14715, #16220, #1224, #2524, #4529, #9748, #12628, #5386, #792, #248, #3904, #4562, #13708, #4367, #13052, #7187, #11623, #16026, #6644, #5812, #12131, #10093, #3286, #13601, #13660, #10340, #13898, #7502, #17008, #14142, #10827, #6449, #8259, #3659, #4620, #5448, #16513, #1276, #12774, #12899, #7776, #17063, #12679, #17497, #11566, #4892, #3097, #9739, #8287, #13230, #16316, #14689, #9429, #882, #13111, #15835, #9703, #11699, #16619, #15517, #7312, #33, #6593, #11586, #12738, #5761, #522 ) ) ;
#1869 = FACE_OUTER_BOUND ( 'NONE', #11982, .T. ) ;
#1870 = CIRCLE ( 'NONE', #12604, 2.500000000000000444 ) ;
#1871 = VERTEX_POINT ( 'NONE', #2360 ) ;
#1872 = VECTOR ( 'NONE', #8173, 1000.000000000000000 ) ;
#1873 = DIRECTION ( 'NONE',  ( -1.000000000000000000, 0.000000000000000000, 0.000000000000000000 ) ) ;
#1874 = CARTESIAN_POINT ( 'NONE',  ( -7.379000772445021283, 18.00000000000000000, 25.00000000000000355 ) ) ;
#1875 = FACE_OUTER_BOUND ( 'NONE', #4435, .T. ) ;
#1876 = DIRECTION ( 'NONE',  ( -0.000000000000000000, -1.000000000000000000, 0.000000000000000000 ) ) ;
#1877 = CARTESIAN_POINT ( 'NONE',  ( -7.379000772444995526, 18.00000000000000000, 25.00000000000000000 ) ) ;
#1878 = DIRECTION ( 'NONE',  ( -1.000000000000000000, 0.000000000000000000, 0.000000000000000000 ) ) ;
#1879 = AXIS2_PLACEMENT_3D ( 'NONE', #17279, #5151, #3919 ) ;
#1880 = CARTESIAN_POINT ( 'NONE',  ( 48.00000000000000000, 171.6227766016838245, 15.00000337241049131 ) ) ;
#1881 = CIRCLE ( 'NONE', #5844, 5.000000000000000888 ) ;
#1882 = ORIENTED_EDGE ( 'NONE', *, *, #197, .T. ) ;
#1883 = DIRECTION ( 'NONE',  ( 0.000000000000000000, 0.000000000000000000, -1.000000000000000000 ) ) ;
#1884 = ORIENTED_EDGE ( 'NONE', *, *, #9370, .T. ) ;
#1885 = CARTESIAN_POINT ( 'NONE',  ( 27.48361012698968864, 136.6227766016838245, 0.000000000000000000 ) ) ;
#1886 = CARTESIAN_POINT ( 'NONE',  ( 49.99999999999998579, 155.6227766016839098, 12.50000337241049309 ) ) ;
#1887 = ORIENTED_EDGE ( 'NONE', *, *, #1457, .T. ) ;
#1888 = CARTESIAN_POINT ( 'NONE',  ( -50.00000000000000000, 154.3022685259950038, 9.999999999999900524 ) ) ;
#1889 = CARTESIAN_POINT ( 'NONE',  ( 49.99999999999998579, 171.6227766016838245, 10.00000337241048953 ) ) ;
#1890 = CARTESIAN_POINT ( 'NONE',  ( 17.19546515351294147, 126.2270863594749670, 7.189547039408070717 ) ) ;
#1891 = AXIS2_PLACEMENT_3D ( 'NONE', #13371, #6643, #4336 ) ;
#1892 = EDGE_LOOP ( 'NONE', ( #13134, #12511 ) ) ;
#1893 = DIRECTION ( 'NONE',  ( 6.938893903907229364E-16, -0.000000000000000000, -1.000000000000000000 ) ) ;
#1894 = CIRCLE ( 'NONE', #10919, 12.00000000000000000 ) ;
#1895 = DIRECTION ( 'NONE',  ( 0.000000000000000000, 1.000000000000000000, 0.000000000000000000 ) ) ;
#1896 = CIRCLE ( 'NONE', #15172, 2.500000000000002220 ) ;
#1897 = CARTESIAN_POINT ( 'NONE',  ( -50.00000000000000000, 171.6227766016838245, -2.296212748401287183E-15 ) ) ;
#1898 = DIRECTION ( 'NONE',  ( 0.000000000000000000, 0.000000000000000000, -1.000000000000000000 ) ) ;
#1899 = ADVANCED_FACE ( 'NONE', ( #1035 ), #13080, .T. ) ;
#1900 = CARTESIAN_POINT ( 'NONE',  ( 17.75267852353177034, 29.94338869414745830, 12.49131726690029254 ) ) ;
#1901 = CARTESIAN_POINT ( 'NONE',  ( -103.0000000000000142, 171.6227766016838245, 25.69059892324149175 ) ) ;
#1902 = VERTEX_POINT ( 'NONE', #2277 ) ;
#1903 = DIRECTION ( 'NONE',  ( -1.000000000000000000, 0.000000000000000000, 0.000000000000000000 ) ) ;
#1904 = LINE ( 'NONE', #9686, #15577 ) ;
#1905 = EDGE_LOOP ( 'NONE', ( #3437, #5081, #4944 ) ) ;
#1906 = DIRECTION ( 'NONE',  ( 0.000000000000000000, 0.000000000000000000, -1.000000000000000000 ) ) ;
#1907 = FACE_BOUND ( 'NONE', #613, .T. ) ;
#1908 = ORIENTED_EDGE ( 'NONE', *, *, #7738, .T. ) ;
#1909 = ORIENTED_EDGE ( 'NONE', *, *, #7068, .F. ) ;
#1910 = CARTESIAN_POINT ( 'NONE',  ( 10.58901158398830766, 139.9616134764785329, 11.54438095561596000 ) ) ;
#1911 = ORIENTED_EDGE ( 'NONE', *, *, #8044, .T. ) ;
#1912 = DIRECTION ( 'NONE',  ( -1.000000000000000000, -0.000000000000000000, 0.000000000000000000 ) ) ;
#1913 = ORIENTED_EDGE ( 'NONE', *, *, #11163, .F. ) ;
#1914 = FILL_AREA_STYLE_COLOUR ( '', #12928 ) ;
#1915 = CARTESIAN_POINT ( 'NONE',  ( 22.50000000000001421, 146.6227766016838245, -21.54065922853802562 ) ) ;
#1916 = CARTESIAN_POINT ( 'NONE',  ( 15.53715976346056493, 125.3980538582347748, 5.670872899454017180 ) ) ;
#1917 = LINE ( 'NONE', #1828, #8747 ) ;
#1918 = EDGE_CURVE ( 'NONE', #4489, #16184, #15822, .T. ) ;
#1919 = EDGE_CURVE ( 'NONE', #7945, #11482, #11675, .T. ) ;
#1920 = CARTESIAN_POINT ( 'NONE',  ( 37.04838423995397534, 144.0140295085317064, -18.09598853029519105 ) ) ;
#1921 = CIRCLE ( 'NONE', #9253, 2.500000000000002220 ) ;
#1922 = EDGE_CURVE ( 'NONE', #3029, #13521, #6943, .T. ) ;
#1923 = AXIS2_PLACEMENT_3D ( 'NONE', #17345, #13283, #11944 ) ;
#1924 = ORIENTED_EDGE ( 'NONE', *, *, #5514, .T. ) ;
#1925 = CARTESIAN_POINT ( 'NONE',  ( 25.53083208230110657, 144.3624319200458785, 18.60312384224725335 ) ) ;
#1926 = LINE ( 'NONE', #14228, #557 ) ;
#1927 = LINE ( 'NONE', #11214, #7366 ) ;
#1928 = CARTESIAN_POINT ( 'NONE',  ( -8.097611523673213796, 19.99999999997653788, -14.83628426572637693 ) ) ;
#1929 = CARTESIAN_POINT ( 'NONE',  ( 36.00000000000002132, 146.6227766016838245, -24.49489742783179125 ) ) ;
#1930 = PRODUCT_DEFINITION_SHAPE ( 'NONE', 'NONE',  #13343 ) ;
#1931 = DIRECTION ( 'NONE',  ( 1.000000000000000000, 0.000000000000000000, 0.000000000000000000 ) ) ;
#1932 = VECTOR ( 'NONE', #6853, 1000.000000000000000 ) ;
#1933 = ORIENTED_EDGE ( 'NONE', *, *, #4250, .F. ) ;
#1934 = DIRECTION ( 'NONE',  ( -1.000000000000000000, 0.000000000000000000, 0.000000000000000000 ) ) ;
#1935 = AXIS2_PLACEMENT_3D ( 'NONE', #13905, #1763, #7161 ) ;
#1936 = ORIENTED_EDGE ( 'NONE', *, *, #13599, .F. ) ;
#1937 = CARTESIAN_POINT ( 'NONE',  ( -86.00000000000005684, 196.3062978594714707, -24.81790219152272670 ) ) ;
#1938 = FACE_OUTER_BOUND ( 'NONE', #299, .T. ) ;
#1939 = PLANE ( 'NONE',  #10931 ) ;
#1940 = ORIENTED_EDGE ( 'NONE', *, *, #11689, .T. ) ;
#1941 = DIRECTION ( 'NONE',  ( -0.000000000000000000, -0.000000000000000000, -1.000000000000000000 ) ) ;
#1942 = FACE_OUTER_BOUND ( 'NONE', #13572, .T. ) ;
#1943 = AXIS2_PLACEMENT_3D ( 'NONE', #8786, #12852, #6124 ) ;
#1944 = DIRECTION ( 'NONE',  ( -1.000000000000000000, 0.000000000000000000, 0.000000000000000000 ) ) ;
#1945 = CIRCLE ( 'NONE', #11827, 33.00000000000000000 ) ;
#1946 = FACE_OUTER_BOUND ( 'NONE', #7383, .T. ) ;
#1947 = ORIENTED_EDGE ( 'NONE', *, *, #3864, .F. ) ;
#1948 = ORIENTED_EDGE ( 'NONE', *, *, #9700, .F. ) ;
#1949 = CARTESIAN_POINT ( 'NONE',  ( 22.45383620668762248, 29.90040889522806111, -11.60055593449971845 ) ) ;
#1950 = CARTESIAN_POINT ( 'NONE',  ( 23.20616110506447072, 140.9816209840972192, -12.26578303444138207 ) ) ;
#1951 = ORIENTED_EDGE ( 'NONE', *, *, #3992, .F. ) ;
#1952 = DIRECTION ( 'NONE',  ( -1.000000000000000000, -0.000000000000000000, 0.000000000000000000 ) ) ;
#1953 = AXIS2_PLACEMENT_3D ( 'NONE', #16994, #6015, #10077 ) ;
#1954 = EDGE_LOOP ( 'NONE', ( #11743, #9542, #6065, #9181 ) ) ;
#1955 = EDGE_CURVE ( 'NONE', #4989, #2572, #9262, .T. ) ;
#1956 = AXIS2_PLACEMENT_3D ( 'NONE', #16087, #3964, #1906 ) ;
#1957 = CARTESIAN_POINT ( 'NONE',  ( 1.559999999999998943, 0.8660254037844428154, 1.500000000000001332 ) ) ;
#1958 = EDGE_CURVE ( 'NONE', #4419, #16184, #4351, .T. ) ;
#1959 = VECTOR ( 'NONE', #5162, 1000.000000000000000 ) ;
#1960 = CARTESIAN_POINT ( 'NONE',  ( -14.54670497998689171, 17.99999999999999645, 23.76610458325318831 ) ) ;
#1961 = CARTESIAN_POINT ( 'NONE',  ( -50.00000000000000000, 204.6227766016838245, -2.020667218593133100E-15 ) ) ;
#1962 = CARTESIAN_POINT ( 'NONE',  ( -206.8291083847463767, 174.6458110457699320, 3.997382128395213563 ) ) ;
#1963 = CARTESIAN_POINT ( 'NONE',  ( -15.84134677353521070, 32.63429591450738343, 7.614689697697072823 ) ) ;
#1964 = CARTESIAN_POINT ( 'NONE',  ( -32.14917720409752633, 119.8847850876495471, 5.472305571546614900 ) ) ;
#1965 = EDGE_CURVE ( 'NONE', #11878, #1245, #15252, .T. ) ;
#1966 = DIRECTION ( 'NONE',  ( -0.000000000000000000, -0.000000000000000000, -1.000000000000000000 ) ) ;
#1967 = VERTEX_POINT ( 'NONE', #14492 ) ;
#1968 = DIRECTION ( 'NONE',  ( -0.000000000000000000, -1.000000000000000000, -0.000000000000000000 ) ) ;
#1969 = EDGE_CURVE ( 'NONE', #1803, #9465, #6493, .T. ) ;
#1970 = VECTOR ( 'NONE', #3890, 1000.000000000000000 ) ;
#1971 = EDGE_LOOP ( 'NONE', ( #2339, #6500, #6406, #10517 ) ) ;
#1972 = LINE ( 'NONE', #9934, #8169 ) ;
#1973 = CIRCLE ( 'NONE', #8755, 5.000000000000000888 ) ;
#1974 = DIRECTION ( 'NONE',  ( 0.000000000000000000, 0.000000000000000000, -1.000000000000000000 ) ) ;
#1975 = ORIENTED_EDGE ( 'NONE', *, *, #7736, .T. ) ;
#1976 = CARTESIAN_POINT ( 'NONE',  ( 27.15273249069231198, 19.99999999999999645, 20.88767039909325973 ) ) ;
#1977 = CARTESIAN_POINT ( 'NONE',  ( 21.59801423301730239, 20.00000000000000000, 12.60094170202890140 ) ) ;
#1978 = DIRECTION ( 'NONE',  ( 1.000000000000000000, 0.000000000000000000, 0.000000000000000000 ) ) ;
#1979 = EDGE_CURVE ( 'NONE', #5635, #9188, #7587, .T. ) ;
#1980 = VECTOR ( 'NONE', #3970, 1000.000000000000000 ) ;
#1981 = VECTOR ( 'NONE', #15313, 1000.000000000000000 ) ;
#1982 = ORIENTED_EDGE ( 'NONE', *, *, #16978, .F. ) ;
#1983 = CONTEXT_DEPENDENT_SHAPE_REPRESENTATION ( #4382, #12816 ) ;
#1984 = DIRECTION ( 'NONE',  ( -1.000000000000000000, 0.000000000000000000, 0.000000000000000000 ) ) ;
#1985 = CIRCLE ( 'NONE', #5948, 20.00000000000000355 ) ;
#1986 = CARTESIAN_POINT ( 'NONE',  ( -27.99999999999998224, 10.00000000000000000, 0.000000000000000000 ) ) ;
#1987 = CARTESIAN_POINT ( 'NONE',  ( -79.59850409272017657, 191.6349927435749692, 26.23951396249187340 ) ) ;
#1988 = EDGE_CURVE ( 'NONE', #14929, #13466, #5112, .T. ) ;
#1989 = CARTESIAN_POINT ( 'NONE',  ( -7.379000772444994638, 20.00000000000000000, 25.00000000000000000 ) ) ;
#1990 = DIRECTION ( 'NONE',  ( -1.000000000000000000, -0.000000000000000000, -0.000000000000000000 ) ) ;
#1991 = DIRECTION ( 'NONE',  ( 0.000000000000000000, 0.000000000000000000, 1.000000000000000000 ) ) ;
#1992 = EDGE_CURVE ( 'NONE', #14157, #15093, #16951, .T. ) ;
#1993 = EDGE_CURVE ( 'NONE', #17220, #3796, #3393, .T. ) ;
#1994 = ORIENTED_EDGE ( 'NONE', *, *, #13315, .T. ) ;
#1995 = CARTESIAN_POINT ( 'NONE',  ( -20.00000000000000355, 171.6227766016838245, 19.49999999999998934 ) ) ;
#1996 = DIRECTION ( 'NONE',  ( -1.000000000000000000, -0.000000000000000000, 0.000000000000000000 ) ) ;
#1997 = ORIENTED_EDGE ( 'NONE', *, *, #14906, .T. ) ;
#1998 = CARTESIAN_POINT ( 'NONE',  ( -72.50000000000000000, 196.6227766016838245, -35.00200000000000244 ) ) ;
#1999 = LINE ( 'NONE', #585, #12329 ) ;
#2000 = AXIS2_PLACEMENT_3D ( 'NONE', #12733, #11043, #8650 ) ;
#2001 = ORIENTED_EDGE ( 'NONE', *, *, #16740, .T. ) ;
#2002 = VERTEX_POINT ( 'NONE', #6264 ) ;
#2003 = EDGE_LOOP ( 'NONE', ( #342, #15510, #2783, #16048 ) ) ;
#2004 = AXIS2_PLACEMENT_3D ( 'NONE', #16969, #3501, #1746 ) ;
#2005 = EDGE_CURVE ( 'NONE', #11482, #7945, #1973, .T. ) ;
#2006 = ORIENTED_EDGE ( 'NONE', *, *, #3078, .T. ) ;
#2007 = ORIENTED_EDGE ( 'NONE', *, *, #6851, .F. ) ;
#2008 = CARTESIAN_POINT ( 'NONE',  ( -45.00000000000000711, 171.6227766016838245, -5.000000000000007994 ) ) ;
#2009 = SURFACE_STYLE_USAGE ( .BOTH. , #15288 ) ;
#2010 = DIRECTION ( 'NONE',  ( 1.000000000000000000, 0.000000000000000000, 0.000000000000000000 ) ) ;
#2011 = AXIS2_PLACEMENT_3D ( 'NONE', #636, #9923, #3019 ) ;
#2012 = B_SPLINE_CURVE_WITH_KNOTS ( 'NONE', 3,
 ( #7126, #13437, #12202, #2462, #3047, #13264, #5392, #14768, #6624, #16106, #13354, #7949, #3982, #6715, #2725, #16192, #12114, #12015, #2559, #14844, #8452, #1218, #6809, #9272, #17418, #6539 ),
 .UNSPECIFIED., .F., .F.,
 ( 4, 2, 2, 2, 2, 2, 2, 2, 2, 2, 2, 2, 4 ),
 ( 0.000000000000000000, 0.002002783134349993537, 0.004005566268699987074, 0.008011132537399970679, 0.01001391567174996812, 0.01201669880609996383, 0.01602226507479994830, 0.01802504820914994227, 0.02002783134349994318, 0.02403339761219993459, 0.02603618074654993550, 0.02803896388089993641, 0.03204453014959993129 ),
 .UNSPECIFIED. ) ;
#2013 = CARTESIAN_POINT ( 'NONE',  ( 25.00000000000000000, 196.6227766016838245, -35.00200000000000244 ) ) ;
#2014 = ORIENTED_EDGE ( 'NONE', *, *, #3196, .T. ) ;
#2015 = CARTESIAN_POINT ( 'NONE',  ( 34.86532646282766024, 145.4324535730256684, 20.08206597984641917 ) ) ;
#2016 = CARTESIAN_POINT ( 'NONE',  ( -73.00000000000001421, 171.6227766016838245, 19.49999999999999645 ) ) ;
#2017 = FACE_BOUND ( 'NONE', #3086, .T. ) ;
#2018 = CARTESIAN_POINT ( 'NONE',  ( -17.59086657693882927, 19.99999999999999645, -22.42595686383492293 ) ) ;
#2019 = CIRCLE ( 'NONE', #4851, 2.500000000000000000 ) ;
#2020 = FACE_OUTER_BOUND ( 'NONE', #13499, .T. ) ;
#2021 = ADVANCED_FACE ( 'NONE', ( #14578 ), #2450, .T. ) ;
#2022 = EDGE_CURVE ( 'NONE', #1170, #5007, #4928, .T. ) ;
#2023 = ADVANCED_FACE ( 'NONE', ( #13259 ), #1128, .F. ) ;
#2024 = ORIENTED_EDGE ( 'NONE', *, *, #10632, .T. ) ;
#2025 = CARTESIAN_POINT ( 'NONE',  ( -100.0000000000000000, 171.6227766016838245, 0.000000000000000000 ) ) ;
#2026 = ORIENTED_EDGE ( 'NONE', *, *, #9908, .T. ) ;
#2027 = CARTESIAN_POINT ( 'NONE',  ( 27.41872110558518116, 136.9783011792879392, 5.130391642808777242 ) ) ;
#2028 = DIRECTION ( 'NONE',  ( 0.8660254037844378194, -0.5000000000000015543, -0.000000000000000000 ) ) ;
#2029 = DIRECTION ( 'NONE',  ( 0.000000000000000000, 1.000000000000000000, 0.000000000000000000 ) ) ;
#2030 = ORIENTED_EDGE ( 'NONE', *, *, #3884, .T. ) ;
#2031 = CARTESIAN_POINT ( 'NONE',  ( -95.00000000000000000, 171.6227766016838245, 27.69059892324149530 ) ) ;
#2032 = DIRECTION ( 'NONE',  ( -1.000000000000000000, 0.000000000000000000, 0.000000000000000000 ) ) ;
#2033 = CARTESIAN_POINT ( 'NONE',  ( 196.0000000000000000, 175.6227766016838530, -21.92820660268601074 ) ) ;
#2034 = CARTESIAN_POINT ( 'NONE',  ( 32.00249589297860808, 202.2831825963720007, -16.88100368216889180 ) ) ;
#2035 = ORIENTED_EDGE ( 'NONE', *, *, #16198, .F. ) ;
#2036 =( BOUNDED_CURVE ( )  B_SPLINE_CURVE ( 3, ( #15011, #2884, #8276, #13685 ),
 .UNSPECIFIED., .F., .F. ) 
 B_SPLINE_CURVE_WITH_KNOTS ( ( 4, 4 ),
 ( -8.881784197001252323E-16, 1.570796326794898556 ),
 .UNSPECIFIED. ) 
 CURVE ( )  GEOMETRIC_REPRESENTATION_ITEM ( )  RATIONAL_B_SPLINE_CURVE ( ( 1.000000000000000000, 0.8047378541243643824, 0.8047378541243643824, 1.000000000000000000 ) ) 
 REPRESENTATION_ITEM ( '' )  );
#2037 = ORIENTED_EDGE ( 'NONE', *, *, #13494, .F. ) ;
#2038 = CARTESIAN_POINT ( 'NONE',  ( 17.53130567297317910, 19.99999999999999289, -14.69383831151754727 ) ) ;
#2039 = CARTESIAN_POINT ( 'NONE',  ( 24.26130280265436667, 140.5733633045254578, -11.19213049117091785 ) ) ;
#2040 = ADVANCED_FACE ( 'NONE', ( #12516 ), #12338, .F. ) ;
#2041 = ORIENTED_EDGE ( 'NONE', *, *, #7584, .T. ) ;
#2042 = FACE_OUTER_BOUND ( 'NONE', #14630, .T. ) ;
#2043 = CARTESIAN_POINT ( 'NONE',  ( -27.99999999999998224, 10.00000000000000000, 0.000000000000000000 ) ) ;
#2044 = VERTEX_POINT ( 'NONE', #13857 ) ;
#2045 = CARTESIAN_POINT ( 'NONE',  ( -154.9692839938123257, 171.6227766016838245, 0.000000000000000000 ) ) ;
#2046 = UNCERTAINTY_MEASURE_WITH_UNIT (LENGTH_MEASURE( 1.000000000000000082E-05 ), #7499, 'distance_accuracy_value', 'NONE');
#2047 = CARTESIAN_POINT ( 'NONE',  ( -31.66708739526795924, 101.0000000000000142, 5.500000000000000000 ) ) ;
#2048 = CARTESIAN_POINT ( 'NONE',  ( 30.00000000000000355, 196.6227766016838245, -35.00000000000000000 ) ) ;
#2049 = CARTESIAN_POINT ( 'NONE',  ( -21.36854569161881301, 18.00000000000000000, 19.70709815271291632 ) ) ;
#2050 = DIRECTION ( 'NONE',  ( -1.156482317317868274E-16, 1.000000000000000000, 0.000000000000000000 ) ) ;
#2051 = CARTESIAN_POINT ( 'NONE',  ( 34.07201977579011043, 142.2001748967346657, -18.96071578072433184 ) ) ;
#2052 = ORIENTED_EDGE ( 'NONE', *, *, #13053, .F. ) ;
#2053 = CARTESIAN_POINT ( 'NONE',  ( 30.49999999999998224, 9.999999999999998224, 10.00000000000000178 ) ) ;
#2054 = ORIENTED_EDGE ( 'NONE', *, *, #12667, .T. ) ;
#2055 = EDGE_CURVE ( 'NONE', #8718, #8018, #5970, .T. ) ;
#2056 = CARTESIAN_POINT ( 'NONE',  ( 1.559999999999998943, -1.732050807568885631, 0.000000000000000000 ) ) ;
#2057 = CYLINDRICAL_SURFACE ( 'NONE', #12618, 5.000000000000004441 ) ;
#2058 = EDGE_LOOP ( 'NONE', ( #1778, #886 ) ) ;
#2059 = DIRECTION ( 'NONE',  ( 0.000000000000000000, 0.000000000000000000, 1.000000000000000000 ) ) ;
#2060 = CARTESIAN_POINT ( 'NONE',  ( 19.38030756396766563, 20.00000000000227018, 14.02844645440659654 ) ) ;
#2061 = CARTESIAN_POINT ( 'NONE',  ( 17.03671980602049985, 126.4628225884666932, 7.681944018317823364 ) ) ;
#2062 = VERTEX_POINT ( 'NONE', #1889 ) ;
#2063 = DIRECTION ( 'NONE',  ( -1.000000000000000000, 0.000000000000000000, 0.000000000000000000 ) ) ;
#2064 = CARTESIAN_POINT ( 'NONE',  ( -83.41681137195966755, 192.9554221994868044, 25.17938093289616575 ) ) ;
#2065 = CARTESIAN_POINT ( 'NONE',  ( -8.730345434444062747, 30.30576128541687453, -14.94291915632153334 ) ) ;
#2066 = CARTESIAN_POINT ( 'NONE',  ( -45.00000000000000000, 136.6227766016838245, 0.000000000000000000 ) ) ;
#2067 = PRODUCT_DEFINITION_SHAPE ( 'NONE', 'NONE',  #17535 ) ;
#2068 = DIRECTION ( 'NONE',  ( 0.000000000000000000, 0.000000000000000000, -1.000000000000000000 ) ) ;
#2069 = ORIENTED_EDGE ( 'NONE', *, *, #1865, .F. ) ;
#2070 = DIRECTION ( 'NONE',  ( -0.000000000000000000, -0.000000000000000000, -1.000000000000000000 ) ) ;
#2071 = CARTESIAN_POINT ( 'NONE',  ( -21.35874126517689930, 20.00000000000000000, -19.71585776365618869 ) ) ;
#2072 = ORIENTED_EDGE ( 'NONE', *, *, #8190, .F. ) ;
#2073 = EDGE_CURVE ( 'NONE', #919, #14342, #2530, .T. ) ;
#2074 = DIRECTION ( 'NONE',  ( -1.000000000000000000, -0.000000000000000000, -0.000000000000000000 ) ) ;
#2075 = CARTESIAN_POINT ( 'NONE',  ( 30.00000000000001066, 146.6227766016838245, -13.00000000000000000 ) ) ;
#2076 = ORIENTED_EDGE ( 'NONE', *, *, #2779, .F. ) ;
#2077 = EDGE_LOOP ( 'NONE', ( #16454, #10005, #10809, #13155, #15622, #14602, #921 ) ) ;
#2078 = ORIENTED_EDGE ( 'NONE', *, *, #17126, .F. ) ;
#2079 = EDGE_CURVE ( 'NONE', #16820, #5595, #3132, .T. ) ;
#2080 = CARTESIAN_POINT ( 'NONE',  ( 30.00000000000000355, 196.6227766016838245, 10.00000000000000178 ) ) ;
#2081 = EDGE_CURVE ( 'NONE', #14731, #11875, #1723, .T. ) ;
#2082 = ORIENTED_EDGE ( 'NONE', *, *, #6415, .T. ) ;
#2083 = CARTESIAN_POINT ( 'NONE',  ( 24.40238044657793992, 141.6105225557631115, -13.74486639216963368 ) ) ;
#2084 = CARTESIAN_POINT ( 'NONE',  ( 6.803110712587624676, 134.0269829078799262, 12.98040381008119759 ) ) ;
#2085 = CARTESIAN_POINT ( 'NONE',  ( 49.99999999999998579, 155.6227766016839098, 12.50000337241049309 ) ) ;
#2086 = CARTESIAN_POINT ( 'NONE',  ( 13.65319468154008042, 138.6827642936709424, 2.302653601763912761 ) ) ;
#2087 = ORIENTED_EDGE ( 'NONE', *, *, #15388, .F. ) ;
#2088 = FACE_OUTER_BOUND ( 'NONE', #403, .T. ) ;
#2089 = CARTESIAN_POINT ( 'NONE',  ( 27.50000000000001066, 146.6227766016838245, -16.00000000000000000 ) ) ;
#2090 = DIRECTION ( 'NONE',  ( -0.000000000000000000, -0.000000000000000000, -1.000000000000000000 ) ) ;
#2091 = B_SPLINE_CURVE_WITH_KNOTS ( 'NONE', 3,
 ( #9558, #1246, #6653, #9209, #4011, #13, #17453, #7886, #6746, #14616, #13559, #6566, #15943, #12224, #3916, #13467, #5495, #4172, #5418, #16034, #95, #12142 ),
 .UNSPECIFIED., .F., .F.,
 ( 4, 2, 2, 2, 2, 2, 2, 2, 2, 2, 4 ),
 ( 0.000000000000000000, 0.002375333402909271790, 0.004750666805818540978, 0.007126000208727810599, 0.009501333611637081955, 0.01068900031309169378, 0.01187666701454630908, 0.01425200041745553273, 0.01543966711891012200, 0.01662733382036471128, 0.01900266722327392452 ),
 .UNSPECIFIED. ) ;
#2092 = CARTESIAN_POINT ( 'NONE',  ( -14.24512928960374225, 19.99999999999770139, -9.752520130898352235 ) ) ;
#2093 = PLANE ( 'NONE',  #12038 ) ;
#2094 = FACE_OUTER_BOUND ( 'NONE', #9674, .T. ) ;
#2095 = VERTEX_POINT ( 'NONE', #7116 ) ;
#2096 = LINE ( 'NONE', #16729, #17441 ) ;
#2097 = VECTOR ( 'NONE', #15350, 1000.000000000000000 ) ;
#2098 = ORIENTED_EDGE ( 'NONE', *, *, #8388, .F. ) ;
#2099 =( NAMED_UNIT ( * ) SI_UNIT ( $, .STERADIAN. ) SOLID_ANGLE_UNIT ( ) );
#2100 = CARTESIAN_POINT ( 'NONE',  ( 48.00000000000000711, 191.6227766016837677, -3.071800142134975431 ) ) ;
#2101 = AXIS2_PLACEMENT_3D ( 'NONE', #11436, #7542, #11616 ) ;
#2102 = CARTESIAN_POINT ( 'NONE',  ( -206.3689767832464668, 173.6103877383153247, 4.531616471133065538 ) ) ;
#2103 = PLANE ( 'NONE',  #7180 ) ;
#2104 = ORIENTED_EDGE ( 'NONE', *, *, #6682, .T. ) ;
#2105 = DIRECTION ( 'NONE',  ( 0.000000000000000000, -1.000000000000000000, 0.000000000000000000 ) ) ;
#2106 = CARTESIAN_POINT ( 'NONE',  ( -725.0000000000000000, 19.99999999999995737, 4.999999999999999112 ) ) ;
#2107 = EDGE_CURVE ( 'NONE', #6775, #938, #14139, .T. ) ;
#2108 = EDGE_CURVE ( 'NONE', #11290, #14157, #14407, .T. ) ;
#2109 = FACE_OUTER_BOUND ( 'NONE', #16606, .T. ) ;
#2110 = CARTESIAN_POINT ( 'NONE',  ( 27.60418301405396235, 202.1282835878848800, -17.15932559113868905 ) ) ;
#2111 = CIRCLE ( 'NONE', #5222, 108.0000000000000142 ) ;
#2112 = ORIENTED_EDGE ( 'NONE', *, *, #4056, .T. ) ;
#2113 = VECTOR ( 'NONE', #4048, 1000.000000000000000 ) ;
#2114 = ORIENTED_EDGE ( 'NONE', *, *, #7525, .F. ) ;
#2115 = CARTESIAN_POINT ( 'NONE',  ( 19.08196460475218714, 19.99999999999773337, -14.16502029867040235 ) ) ;
#2116 = CYLINDRICAL_SURFACE ( 'NONE', #9223, 750.0000000000001137 ) ;
#2117 = EDGE_LOOP ( 'NONE', ( #2692, #12862 ) ) ;
#2118 = CYLINDRICAL_SURFACE ( 'NONE', #8106, 5.000000000000004441 ) ;
#2119 = CARTESIAN_POINT ( 'NONE',  ( 6.134011831684059501, 140.6204725398426092, -12.99999999999999822 ) ) ;
#2120 = ORIENTED_EDGE ( 'NONE', *, *, #1162, .F. ) ;
#2121 = DIRECTION ( 'NONE',  ( 1.000000000000000000, 0.000000000000000000, -0.000000000000000000 ) ) ;
#2122 = VECTOR ( 'NONE', #14100, 1000.000000000000114 ) ;
#2123 = AXIS2_PLACEMENT_3D ( 'NONE', #9388, #10806, #4260 ) ;
#2124 = AXIS2_PLACEMENT_3D ( 'NONE', #8738, #12629, #5732 ) ;
#2125 = CARTESIAN_POINT ( 'NONE',  ( -87.50000000000004263, 146.6227766016838245, -13.00000000000000000 ) ) ;
#2126 = CARTESIAN_POINT ( 'NONE',  ( 1.559999999999998943, 0.8660254037844428154, 1.500000000000001332 ) ) ;
#2127 = CARTESIAN_POINT ( 'NONE',  ( -12.35971836118926959, 18.00000000000229861, 8.238707107740440350 ) ) ;
#2128 = ADVANCED_FACE ( 'NONE', ( #8344 ), #464, .F. ) ;
#2129 = ADVANCED_FACE ( 'NONE', ( #304 ), #7196, .T. ) ;
#2130 = CARTESIAN_POINT ( 'NONE',  ( -138.7106781186547266, 171.6227766016838245, -25.00000000000000000 ) ) ;
#2131 = ADVANCED_FACE ( 'NONE', ( #11267 ), #1473, .F. ) ;
#2132 = EDGE_CURVE ( 'NONE', #16060, #12961, #14037, .T. ) ;
#2133 = CARTESIAN_POINT ( 'NONE',  ( -27.99999999999998224, 10.00000000000000000, -35.00000000000000000 ) ) ;
#2134 = VERTEX_POINT ( 'NONE', #8529 ) ;
#2135 = DIRECTION ( 'NONE',  ( 0.000000000000000000, 0.000000000000000000, -1.000000000000000000 ) ) ;
#2136 = VERTEX_POINT ( 'NONE', #13938 ) ;
#2137 = CARTESIAN_POINT ( 'NONE',  ( 196.0000000000000000, 187.6227766016837961, -15.00000337241049486 ) ) ;
#2138 = VECTOR ( 'NONE', #8112, 1000.000000000000000 ) ;
#2139 = DIRECTION ( 'NONE',  ( -1.000000000000000000, 0.000000000000000000, 0.000000000000000000 ) ) ;
#2140 = CIRCLE ( 'NONE', #1853, 39.99999999999997868 ) ;
#2141 = VERTEX_POINT ( 'NONE', #1801 ) ;
#2142 = CARTESIAN_POINT ( 'NONE',  ( -40.00000000000000000, 4.000000000000007105, 30.00000000000000711 ) ) ;
#2143 = CARTESIAN_POINT ( 'NONE',  ( 33.66001102075547635, 19.99999999999999645, 12.05479157725600459 ) ) ;
#2144 = VERTEX_POINT ( 'NONE', #4204 ) ;
#2145 = EDGE_CURVE ( 'NONE', #1902, #17455, #2219, .T. ) ;
#2146 = DIRECTION ( 'NONE',  ( -1.000000000000000000, -0.000000000000000000, -0.000000000000000000 ) ) ;
#2147 = CLOSED_SHELL ( 'NONE', ( #14473, #16622, #2895, #16851, #8239, #12846 ) ) ;
#2148 = CARTESIAN_POINT ( 'NONE',  ( -79.79487623779336047, 191.6231342001797771, 26.24853702829032542 ) ) ;
#2149 = CARTESIAN_POINT ( 'NONE',  ( -9.725435201701724708, 30.52647059548997888, -14.77261045527475147 ) ) ;
#2150 = DIRECTION ( 'NONE',  ( 0.000000000000000000, 0.000000000000000000, -1.000000000000000000 ) ) ;
#2151 = AXIS2_PLACEMENT_3D ( 'NONE', #14988, #10829, #1365 ) ;
#2152 = DIRECTION ( 'NONE',  ( 0.000000000000000000, 0.000000000000000000, 1.000000000000000000 ) ) ;
#2153 = ORIENTED_EDGE ( 'NONE', *, *, #13026, .T. ) ;
#2154 = CARTESIAN_POINT ( 'NONE',  ( -7.379000772444994638, 30.00000000000000000, -15.00000000000000000 ) ) ;
#2155 = CARTESIAN_POINT ( 'NONE',  ( -25.81010901361623056, 20.00000000000000000, -13.97188021846430850 ) ) ;
#2156 = EDGE_LOOP ( 'NONE', ( #8329, #5068, #5967, #8726 ) ) ;
#2157 = DIRECTION ( 'NONE',  ( 0.000000000000000000, 0.000000000000000000, 1.000000000000000000 ) ) ;
#2158 = LINE ( 'NONE', #15696, #16584 ) ;
#2159 = EDGE_LOOP ( 'NONE', ( #192, #9491, #3409, #5257, #559 ) ) ;
#2160 = ORIENTED_EDGE ( 'NONE', *, *, #9048, .T. ) ;
#2161 = AXIS2_PLACEMENT_3D ( 'NONE', #1169, #9304, #17459 ) ;
#2162 = AXIS2_PLACEMENT_3D ( 'NONE', #11423, #7100, #7179 ) ;
#2163 = CIRCLE ( 'NONE', #3012, 35.00000000000000000 ) ;
#2165 = CARTESIAN_POINT ( 'NONE',  ( -79.69361278289508732, 154.1221233254128720, -27.97726104294734029 ) ) ;
#2164 = PRESENTATION_LAYER_ASSIGNMENT (  '', '', ( #12110 ) ) ;
#2166 = CIRCLE ( 'NONE', #14325, 747.9999999999998863 ) ;
#2167 = ORIENTED_EDGE ( 'NONE', *, *, #4621, .T. ) ;
#2168 = ADVANCED_FACE ( 'NONE', ( #4811 ), #14803, .F. ) ;
#2169 = CARTESIAN_POINT ( 'NONE',  ( -13.00560346926692645, 31.78932620563996281, 11.23370548922391521 ) ) ;
#2170 = EDGE_CURVE ( 'NONE', #14731, #13379, #277, .T. ) ;
#2171 = DIRECTION ( 'NONE',  ( -1.156482317317868274E-16, 1.000000000000000000, 0.000000000000000000 ) ) ;
#2172 = CARTESIAN_POINT ( 'NONE',  ( 49.99999999999998579, 183.6227766016837961, 5.571800142134975431 ) ) ;
#2173 = DIRECTION ( 'NONE',  ( 1.000000000000000000, 0.000000000000000000, 8.673617379884037937E-17 ) ) ;
#2174 = CARTESIAN_POINT ( 'NONE',  ( 48.00000000000000711, 179.6227766016838245, -12.50000337241049309 ) ) ;
#2175 = ORIENTED_EDGE ( 'NONE', *, *, #5274, .F. ) ;
#2176 = DIRECTION ( 'NONE',  ( 0.000000000000000000, 0.000000000000000000, 1.000000000000000000 ) ) ;
#2177 = CARTESIAN_POINT ( 'NONE',  ( -95.00000000000000000, 171.6227766016838245, -25.69059892324149175 ) ) ;
#2178 = CIRCLE ( 'NONE', #6713, 6.000000000000005329 ) ;
#2179 = CARTESIAN_POINT ( 'NONE',  ( 34.99999999999999289, -20.00000000000000000, -40.00000000000001421 ) ) ;
#2180 = CARTESIAN_POINT ( 'NONE',  ( 24.87028194210262910, 29.86925052300016858, 6.309743549972420595 ) ) ;
#2181 = DIRECTION ( 'NONE',  ( 1.000000000000000000, 1.156482317317868274E-16, -0.000000000000000000 ) ) ;
#2182 = ADVANCED_FACE ( 'NONE', ( #2767 ), #7800, .T. ) ;
#2183 = CARTESIAN_POINT ( 'NONE',  ( 30.90732076053024002, 201.5450689758320095, 13.91624649103840206 ) ) ;
#2184 = ORIENTED_EDGE ( 'NONE', *, *, #10068, .T. ) ;
#2185 = PRESENTATION_STYLE_ASSIGNMENT (( #9357 ) ) ;
#2186 = DIRECTION ( 'NONE',  ( -0.000000000000000000, -0.000000000000000000, -1.000000000000000000 ) ) ;
#2187 = EDGE_LOOP ( 'NONE', ( #14896, #16863, #4548, #13228 ) ) ;
#2188 = FILL_AREA_STYLE ('',( #5926 ) ) ;
#2189 = CIRCLE ( 'NONE', #16051, 20.00000000000000355 ) ;
#2190 = CARTESIAN_POINT ( 'NONE',  ( -103.0000000000000142, 171.6227766016838245, -25.69059892324149175 ) ) ;
#2191 = AXIS2_PLACEMENT_3D ( 'NONE', #4347, #13833, #1699 ) ;
#2192 = AXIS2_PLACEMENT_3D ( 'NONE', #12032, #5215, #12128 ) ;
#2193 = CARTESIAN_POINT ( 'NONE',  ( -34.99999999999999289, 120.0000000000000000, 0.000000000000000000 ) ) ;
#2194 = DIRECTION ( 'NONE',  ( 0.000000000000000000, 1.000000000000000000, 0.000000000000000000 ) ) ;
#2195 = VERTEX_POINT ( 'NONE', #9129 ) ;
#2196 = LINE ( 'NONE', #880, #4743 ) ;
#2197 = DIRECTION ( 'NONE',  ( 1.000000000000000000, 0.000000000000000000, -0.000000000000000000 ) ) ;
#2198 = DIRECTION ( 'NONE',  ( 0.000000000000000000, -0.4999999999999952816, 0.8660254037844413721 ) ) ;
#2199 =( LENGTH_UNIT ( ) NAMED_UNIT ( * ) SI_UNIT ( .MILLI., .METRE. ) );
#2200 = ADVANCED_FACE ( 'NONE', ( #13212 ), #4020, .T. ) ;
#2201 = ORIENTED_EDGE ( 'NONE', *, *, #520, .F. ) ;
#2202 = AXIS2_PLACEMENT_3D ( 'NONE', #17296, #5166, #15531 ) ;
#2203 = ORIENTED_EDGE ( 'NONE', *, *, #12801, .F. ) ;
#2204 = CARTESIAN_POINT ( 'NONE',  ( 19.47274266584531333, 19.99999999999999645, -24.48069943974461538 ) ) ;
#2205 = CIRCLE ( 'NONE', #12109, 10.00000000000000178 ) ;
#2206 = COLOUR_RGB ( '', 0.40784314, 0.44705882, 0.49803922) ;
#2207 = DIRECTION ( 'NONE',  ( 0.000000000000000000, -1.000000000000000000, 0.000000000000000000 ) ) ;
#2208 = VERTEX_POINT ( 'NONE', #16049 ) ;
#2209 = DIRECTION ( 'NONE',  ( -1.000000000000000000, -0.000000000000000000, -0.000000000000000000 ) ) ;
#2210 = DIRECTION ( 'NONE',  ( 0.000000000000000000, 0.000000000000000000, -1.000000000000000000 ) ) ;
#2211 = VERTEX_POINT ( 'NONE', #6388 ) ;
#2212 = EDGE_CURVE ( 'NONE', #3871, #2837, #9312, .T. ) ;
#2213 = DIRECTION ( 'NONE',  ( 1.000000000000000000, 0.000000000000000000, 0.000000000000000000 ) ) ;
#2214 = AXIS2_PLACEMENT_3D ( 'NONE', #3386, #7619, #14523 ) ;
#2215 = VECTOR ( 'NONE', #2028, 1000.000000000000000 ) ;
#2216 = CARTESIAN_POINT ( 'NONE',  ( 39.99999999999997868, 8.000000000000010658, 40.00000000000000711 ) ) ;
#2217 = CARTESIAN_POINT ( 'NONE',  ( -24.94987437106622252, 120.0000000000000284, 6.000000000000001776 ) ) ;
#2218 = CARTESIAN_POINT ( 'NONE',  ( -12.66151707385296987, 17.99999999999770495, 6.998435355972849159 ) ) ;
#2219 = B_SPLINE_CURVE_WITH_KNOTS ( 'NONE', 3,
 ( #1536, #6934, #16431, #4293, #9672, #12860, #3656, #16769, #3398, #8864 ),
 .UNSPECIFIED., .F., .F.,
 ( 4, 2, 2, 2, 4 ),
 ( 0.03775390620236033362, 0.04033669301524714368, 0.04291947982813395374, 0.04550226664102076379, 0.04808505345390757385 ),
 .UNSPECIFIED. ) ;
#2220 = CYLINDRICAL_SURFACE ( 'NONE', #16819, 250.0000000000000000 ) ;
#2221 = CARTESIAN_POINT ( 'NONE',  ( 30.67194674767677753, 140.6591056634353549, -16.31724425057294070 ) ) ;
#2222 = ORIENTED_EDGE ( 'NONE', *, *, #14690, .T. ) ;
#2223 = LINE ( 'NONE', #12944, #11262 ) ;
#2224 = EDGE_LOOP ( 'NONE', ( #692, #3818, #4573, #8253 ) ) ;
#2225 = LINE ( 'NONE', #12854, #3091 ) ;
#2226 = AXIS2_PLACEMENT_3D ( 'NONE', #15939, #7882, #17448 ) ;
#2227 = DIRECTION ( 'NONE',  ( 0.000000000000000000, 0.000000000000000000, 1.000000000000000000 ) ) ;
#2228 =( REPRESENTATION_RELATIONSHIP ('NONE','NONE', #9723, #13460 ) REPRESENTATION_RELATIONSHIP_WITH_TRANSFORMATION ( #9416 )SHAPE_REPRESENTATION_RELATIONSHIP( ) );
#2229 = AXIS2_PLACEMENT_3D ( 'NONE', #2965, #8362, #5374 ) ;
#2230 = ORIENTED_EDGE ( 'NONE', *, *, #15704, .T. ) ;
#2231 = CARTESIAN_POINT ( 'NONE',  ( 24.94691999498327206, 20.00000000000000355, 22.32501294936691139 ) ) ;
#2232 = AXIS2_PLACEMENT_3D ( 'NONE', #17127, #11810, #7925 ) ;
#2233 = CARTESIAN_POINT ( 'NONE',  ( -43.00000000000003553, 134.2062027339443944, -13.00000000000000000 ) ) ;
#2234 = EDGE_CURVE ( 'NONE', #17297, #2257, #15871, .T. ) ;
#2235 = EDGE_CURVE ( 'NONE', #14130, #4871, #3742, .T. ) ;
#2236 = CARTESIAN_POINT ( 'NONE',  ( 30.80964797964808000, 19.99999999999999645, 17.18170494867160514 ) ) ;
#2237 = EDGE_CURVE ( 'NONE', #15620, #3735, #12426, .T. ) ;
#2238 = ORIENTED_EDGE ( 'NONE', *, *, #12023, .F. ) ;
#2239 = DIRECTION ( 'NONE',  ( 0.000000000000000000, 0.000000000000000000, -1.000000000000000000 ) ) ;
#2240 = DIRECTION ( 'NONE',  ( -1.000000000000000000, 0.000000000000000000, 0.000000000000000000 ) ) ;
#2241 = CIRCLE ( 'NONE', #7608, 2.499999999999998668 ) ;
#2242 = CARTESIAN_POINT ( 'NONE',  ( -10.05507621332305668, 30.59909908010286372, -14.70163937327580328 ) ) ;
#2243 = AXIS2_PLACEMENT_3D ( 'NONE', #5868, #9754, #1076 ) ;
#2244 = CARTESIAN_POINT ( 'NONE',  ( -16.41264213764166513, 18.00000000000000000, -23.02790928165778794 ) ) ;
#2245 = ORIENTED_EDGE ( 'NONE', *, *, #12411, .F. ) ;
#2246 = DIRECTION ( 'NONE',  ( -1.000000000000000000, -0.000000000000000000, -0.000000000000000000 ) ) ;
#2247 = ORIENTED_EDGE ( 'NONE', *, *, #5384, .T. ) ;
#2248 = CARTESIAN_POINT ( 'NONE',  ( 31.79926070065823041, 190.8809388003084280, -29.22564348704268511 ) ) ;
#2249 = FACE_BOUND ( 'NONE', #13044, .T. ) ;
#2250 = ORIENTED_EDGE ( 'NONE', *, *, #9908, .F. ) ;
#2251 = ORIENTED_EDGE ( 'NONE', *, *, #4788, .T. ) ;
#2252 = ORIENTED_EDGE ( 'NONE', *, *, #4685, .F. ) ;
#2253 = CIRCLE ( 'NONE', #4530, 11.93698985866628526 ) ;
#2254 = AXIS2_PLACEMENT_3D ( 'NONE', #12118, #6975, #8121 ) ;
#2255 = CARTESIAN_POINT ( 'NONE',  ( -76.92553734538029175, 153.4692325703934728, -27.55849099911372946 ) ) ;
#2256 = VECTOR ( 'NONE', #10322, 1000.000000000000000 ) ;
#2257 = VERTEX_POINT ( 'NONE', #6758 ) ;
#2258 = DIRECTION ( 'NONE',  ( 1.000000000000000000, 0.000000000000000000, 0.000000000000000000 ) ) ;
#2259 = CARTESIAN_POINT ( 'NONE',  ( -16.28901493728125160, 32.76428253546148284, 5.573780508339472028 ) ) ;
#2260 =( NAMED_UNIT ( * ) PLANE_ANGLE_UNIT ( ) SI_UNIT ( $, .RADIAN. ) );
#2261 = LINE ( 'NONE', #17395, #13838 ) ;
#2262 = DIRECTION ( 'NONE',  ( -1.000000000000000000, -0.000000000000000000, 0.000000000000000000 ) ) ;
#2263 = DIRECTION ( 'NONE',  ( 0.9961946980917461003, -0.04357787137382628656, 0.07547908730516766918 ) ) ;
#2264 = EDGE_LOOP ( 'NONE', ( #516, #5165, #2426, #7820 ) ) ;
#2265 = CARTESIAN_POINT ( 'NONE',  ( 26.66247177481912800, 139.4607352144954007, 7.398570892697257761 ) ) ;
#2266 = VECTOR ( 'NONE', #1756, 1000.000000000000000 ) ;
#2267 = AXIS2_PLACEMENT_3D ( 'NONE', #1409, #16276, #6629 ) ;
#2268 = CARTESIAN_POINT ( 'NONE',  ( -100.0000000000000000, 120.0000000000000284, 6.000000000000001776 ) ) ;
#2269 = CARTESIAN_POINT ( 'NONE',  ( 196.0000000000000000, 167.6227766016838814, 19.42820660268601074 ) ) ;
#2270 = CARTESIAN_POINT ( 'NONE',  ( 23.07174175064647059, 29.89240369784053897, 10.82181213433699618 ) ) ;
#2271 = VERTEX_POINT ( 'NONE', #1174 ) ;
#2272 = CARTESIAN_POINT ( 'NONE',  ( 39.99999999999998579, 4.000000000000000000, 30.00000000000001066 ) ) ;
#2273 = ADVANCED_FACE ( 'NONE', ( #7985 ), #13386, .T. ) ;
#2274 = CARTESIAN_POINT ( 'NONE',  ( 25.00000000000000355, 197.2415780845127244, 20.82248078717325157 ) ) ;
#2275 = EDGE_LOOP ( 'NONE', ( #10294, #17016, #12234, #9716 ) ) ;
#2276 = LINE ( 'NONE', #17413, #10935 ) ;
#2277 = CARTESIAN_POINT ( 'NONE',  ( -72.50000000000000000, 196.6227766016838245, -21.54065922853802562 ) ) ;
#2278 = AXIS2_PLACEMENT_3D ( 'NONE', #6951, #14041, #13872 ) ;
#2279 = EDGE_LOOP ( 'NONE', ( #3266, #2377, #8282 ) ) ;
#2280 = CARTESIAN_POINT ( 'NONE',  ( -78.47034442031463186, 141.8580068101642553, 14.25043922611179248 ) ) ;
#2281 = B_SPLINE_CURVE_WITH_KNOTS ( 'NONE', 3,
 ( #6926, #5350, #3942, #204, #9409, #8257, #13492, #6855, #10999, #9666, #5519, #14812, #5610, #11978, #6771, #16061, #8335, #1364, #16157, #12331, #16238, #5252, #12243, #10655, #38, #5437, #115, #16421, #14736, #9323, #4285, #10828, #14900, #8171, #1183, #6588, #17379, #2609, #7994, #15336, #15152, #295, #1793, #11167, #16586, #10008 ),
 .UNSPECIFIED., .F., .F.,
 ( 4, 2, 2, 2, 2, 2, 2, 2, 2, 2, 2, 2, 2, 2, 2, 2, 2, 2, 2, 2, 2, 2, 4 ),
 ( 0.01035378412632265502, 0.01206629175607501145, 0.01377879938582736614, 0.01549130701557972084, 0.01634756083045589559, 0.01720381464533207033, 0.01806006846020824508, 0.01891632227508441982, 0.02062882990483679013, 0.02148508371971297182, 0.02234133753458915350, 0.02319759134946533866, 0.02405384516434152381, 0.02576635279409384555, 0.02747886042384617075, 0.02833511423872235591, 0.02919136805359853412, 0.03090387568335089402, 0.03261638331310325739, 0.03432889094285561382, 0.03604139857260797719, 0.03689765238748415888, 0.03775390620236033362 ),
 .UNSPECIFIED. ) ;
#2282 = AXIS2_PLACEMENT_3D ( 'NONE', #5784, #9767, #16689 ) ;
#2283 = DIRECTION ( 'NONE',  ( 0.000000000000000000, 0.000000000000000000, -1.000000000000000000 ) ) ;
#2284 = CARTESIAN_POINT ( 'NONE',  ( -77.39307936938270416, 141.2146784997055704, -17.33162689407163271 ) ) ;
#2285 = CARTESIAN_POINT ( 'NONE',  ( 49.99999999999998579, 171.6227766016838245, -10.00000337241048953 ) ) ;
#2286 = ORIENTED_EDGE ( 'NONE', *, *, #6993, .T. ) ;
#2287 = CYLINDRICAL_SURFACE ( 'NONE', #8127, 11.99999999999999645 ) ;
#2288 = PLANE ( 'NONE',  #3649 ) ;
#2289 = DIRECTION ( 'NONE',  ( -1.000000000000000000, -0.000000000000000000, -0.000000000000000000 ) ) ;
#2290 = CARTESIAN_POINT ( 'NONE',  ( 26.52485666266940711, 201.5283731665715834, -18.18938113080312391 ) ) ;
#2291 = VERTEX_POINT ( 'NONE', #16146 ) ;
#2292 = AXIS2_PLACEMENT_3D ( 'NONE', #10372, #2325, #14539 ) ;
#2293 = VERTEX_POINT ( 'NONE', #12154 ) ;
#2294 = EDGE_CURVE ( 'NONE', #15865, #14137, #11855, .T. ) ;
#2295 = CARTESIAN_POINT ( 'NONE',  ( 16.23725950538873164, 20.00000000000000000, -24.99999999984155252 ) ) ;
#2296 = CARTESIAN_POINT ( 'NONE',  ( 12.26645298401004425, 138.5600601684519120, -12.85897773338031946 ) ) ;
#2297 = VERTEX_POINT ( 'NONE', #3111 ) ;
#2298 = CARTESIAN_POINT ( 'NONE',  ( -77.01821113640596650, 151.8338245663404678, -28.86895077895843542 ) ) ;
#2299 = CARTESIAN_POINT ( 'NONE',  ( 10.91733900447548322, 143.9222794873857652, -17.93588862913478366 ) ) ;
#2300 = ADVANCED_FACE ( 'NONE', ( #13921 ), #15238, .F. ) ;
#2301 = ORIENTED_EDGE ( 'NONE', *, *, #5852, .T. ) ;
#2302 = CARTESIAN_POINT ( 'NONE',  ( -70.00000000000000000, 171.6227766016838245, 0.000000000000000000 ) ) ;
#2303 = EDGE_CURVE ( 'NONE', #11799, #16546, #836, .T. ) ;
#2304 = EDGE_CURVE ( 'NONE', #4489, #453, #4357, .T. ) ;
#2305 = AXIS2_PLACEMENT_3D ( 'NONE', #16232, #4102, #9485 ) ;
#2306 = CARTESIAN_POINT ( 'NONE',  ( 27.99999999999998224, 9.999999999999998224, 10.00000000000000178 ) ) ;
#2307 = CARTESIAN_POINT ( 'NONE',  ( 196.0000000000000000, 183.6227766016837961, 8.071800142134975431 ) ) ;
#2308 = CARTESIAN_POINT ( 'NONE',  ( 22.93524650466135739, 29.84210526317653489, -5.528689893908154573 ) ) ;
#2309 = CARTESIAN_POINT ( 'NONE',  ( -10.04118010627651181, 18.00000000000000000, 24.87462214922868142 ) ) ;
#2310 = DIRECTION ( 'NONE',  ( -0.000000000000000000, -0.000000000000000000, -1.000000000000000000 ) ) ;
#2311 = DIRECTION ( 'NONE',  ( 1.000000000000000000, 0.000000000000000000, 0.000000000000000000 ) ) ;
#2312 = ORIENTED_EDGE ( 'NONE', *, *, #10648, .F. ) ;
#2313 = DIRECTION ( 'NONE',  ( -1.000000000000000000, -0.000000000000000000, -0.000000000000000000 ) ) ;
#2314 = EDGE_CURVE ( 'NONE', #14544, #10995, #3072, .T. ) ;
#2315 = EDGE_LOOP ( 'NONE', ( #13827, #3262, #5910, #7155, #15380, #5304 ) ) ;
#2316 = CARTESIAN_POINT ( 'NONE',  ( -80.00000000000001421, 196.6227766016838245, -35.00200000000000244 ) ) ;
#2317 = CARTESIAN_POINT ( 'NONE',  ( -38.00000000000000000, 2.000000000000000000, 0.000000000000000000 ) ) ;
#2318 = ORIENTED_EDGE ( 'NONE', *, *, #7734, .F. ) ;
#2319 = CARTESIAN_POINT ( 'NONE',  ( -12.97728802729275088, 19.99999999999883826, 11.64645903342270827 ) ) ;
#2320 = CARTESIAN_POINT ( 'NONE',  ( 10.61972500670372277, 131.6239249143206393, 11.92364046234351527 ) ) ;
#2321 = CARTESIAN_POINT ( 'NONE',  ( 34.93420767853318409, 19.99999999999999645, 5.000000000000010658 ) ) ;
#2322 = ORIENTED_EDGE ( 'NONE', *, *, #9701, .T. ) ;
#2323 = DIRECTION ( 'NONE',  ( -1.000000000000000000, -0.000000000000000000, -0.000000000000000000 ) ) ;
#2324 = CARTESIAN_POINT ( 'NONE',  ( -100.0000000000000000, 144.1839557653416080, 18.33333333333335702 ) ) ;
#2325 = DIRECTION ( 'NONE',  ( 0.000000000000000000, -0.4999999999999952816, -0.8660254037844413721 ) ) ;
#2326 = CARTESIAN_POINT ( 'NONE',  ( -9.480043248728311056, 17.99999999999769784, -11.96743332394513715 ) ) ;
#2327 = ORIENTED_EDGE ( 'NONE', *, *, #3162, .F. ) ;
#2328 = CARTESIAN_POINT ( 'NONE',  ( 1.559999999999998943, -1.299038105676664223, -0.7500000000000006661 ) ) ;
#2329 = EDGE_CURVE ( 'NONE', #11846, #11660, #15586, .T. ) ;
#2330 = ADVANCED_FACE ( 'NONE', ( #14094 ), #5951, .T. ) ;
#2331 = EDGE_CURVE ( 'NONE', #9736, #4487, #9028, .T. ) ;
#2332 = ORIENTED_EDGE ( 'NONE', *, *, #13564, .T. ) ;
#2333 = CARTESIAN_POINT ( 'NONE',  ( -22.99999999999999289, 120.0000000000000142, 0.000000000000000000 ) ) ;
#2334 = DIRECTION ( 'NONE',  ( -1.000000000000000000, -0.000000000000000000, -0.000000000000000000 ) ) ;
#2335 = ORIENTED_EDGE ( 'NONE', *, *, #14223, .T. ) ;
#2336 = VERTEX_POINT ( 'NONE', #634 ) ;
#2337 = EDGE_LOOP ( 'NONE', ( #4983, #602, #8567, #12974 ) ) ;
#2338 = CARTESIAN_POINT ( 'NONE',  ( -83.54345905997189448, 153.2387635573000750, -27.40528370530128299 ) ) ;
#2339 = ORIENTED_EDGE ( 'NONE', *, *, #14502, .F. ) ;
#2340 = DIRECTION ( 'NONE',  ( 0.000000000000000000, 0.000000000000000000, 1.000000000000000000 ) ) ;
#2341 = CARTESIAN_POINT ( 'NONE',  ( -14.26174088910747706, 32.16828253888332512, 10.14247415352539683 ) ) ;
#2342 = CARTESIAN_POINT ( 'NONE',  ( -9.725435201701724708, 30.52647059548997888, 14.77261045527475147 ) ) ;
#2343 = CARTESIAN_POINT ( 'NONE',  ( 37.50000000000000711, 146.6227766016838245, -21.54065922853802562 ) ) ;
#2344 = CARTESIAN_POINT ( 'NONE',  ( 15.00000000000903455, 143.2885527162398489, 16.91661185963483760 ) ) ;
#2345 = CARTESIAN_POINT ( 'NONE',  ( -100.0000000000000000, 143.0439382767972347, 16.49999999999984368 ) ) ;
#2346 = ORIENTED_EDGE ( 'NONE', *, *, #1682, .F. ) ;
#2347 = CARTESIAN_POINT ( 'NONE',  ( 24.75325409605274274, 140.3706687641101212, 10.61653890585399296 ) ) ;
#2348 = CARTESIAN_POINT ( 'NONE',  ( 18.77390920412167929, 29.94862569121198348, -14.25030649093772972 ) ) ;
#2349 = EDGE_CURVE ( 'NONE', #13323, #6602, #10155, .T. ) ;
#2350 = ADVANCED_FACE ( 'NONE', ( #6028, #10348 ), #6283, .F. ) ;
#2351 = DIRECTION ( 'NONE',  ( -1.000000000000000000, 0.000000000000000000, 0.000000000000000000 ) ) ;
#2352 = CARTESIAN_POINT ( 'NONE',  ( 34.93420767853314146, 18.00000000000000355, 6.320602137672510779 ) ) ;
#2353 = CARTESIAN_POINT ( 'NONE',  ( 17.00000000000000000, 206.6227766016838245, 2.143131898507868248E-15 ) ) ;
#2354 = EDGE_CURVE ( 'NONE', #15563, #4664, #11297, .T. ) ;
#2355 = EDGE_LOOP ( 'NONE', ( #14326, #11383, #6376, #8501 ) ) ;
#2356 = DIRECTION ( 'NONE',  ( 0.000000000000000000, 0.000000000000000000, -1.000000000000000000 ) ) ;
#2357 = CARTESIAN_POINT ( 'NONE',  ( -206.3689767832464668, 174.5534660175772785, -3.987129972734268168 ) ) ;
#2358 = VERTEX_POINT ( 'NONE', #15756 ) ;
#2359 = PLANE ( 'NONE',  #14622 ) ;
#2360 = CARTESIAN_POINT ( 'NONE',  ( -70.00000000000000000, 191.6227766016837961, -1.224646799147353454E-15 ) ) ;
#2361 = ORIENTED_EDGE ( 'NONE', *, *, #7591, .T. ) ;
#2362 = SHAPE_REPRESENTATION_RELATIONSHIP ( 'NONE' , 'NONE' ,  #12790, #14383 ) ;
#2363 = CARTESIAN_POINT ( 'NONE',  ( -81.72853406442757773, 141.9273338169157626, 14.39467838667816579 ) ) ;
#2364 = CARTESIAN_POINT ( 'NONE',  ( 14.93242934743710570, 18.00000000000000000, -25.00000000000000000 ) ) ;
#2365 = LINE ( 'NONE', #3883, #4770 ) ;
#2366 = EDGE_CURVE ( 'NONE', #938, #6775, #5074, .T. ) ;
#2367 = CARTESIAN_POINT ( 'NONE',  ( -100.0000000000000000, 201.6227766016838245, 0.000000000000000000 ) ) ;
#2368 = EDGE_LOOP ( 'NONE', ( #953, #11410 ) ) ;
#2369 = CARTESIAN_POINT ( 'NONE',  ( -27.98221281347037959, 30.00000000000000000, -15.00000000000000000 ) ) ;
#2370 = PLANE ( 'NONE',  #14682 ) ;
#2371 = CARTESIAN_POINT ( 'NONE',  ( -50.00000000000000000, 171.6227766016838245, 0.000000000000000000 ) ) ;
#2372 = CARTESIAN_POINT ( 'NONE',  ( 31.06650171500291790, 202.5285685493725794, -16.42664996635052432 ) ) ;
#2373 = ORIENTED_EDGE ( 'NONE', *, *, #6135, .T. ) ;
#2374 = ORIENTED_EDGE ( 'NONE', *, *, #9161, .T. ) ;
#2375 = TOROIDAL_SURFACE ( 'NONE', #9156, -78.75916623668499028, 110.0000000000000142 ) ;
#2376 = VECTOR ( 'NONE', #9308, 1000.000000000000000 ) ;
#2377 = ORIENTED_EDGE ( 'NONE', *, *, #13820, .T. ) ;
#2378 = DIRECTION ( 'NONE',  ( -0.000000000000000000, -0.000000000000000000, 1.000000000000000000 ) ) ;
#2379 = CARTESIAN_POINT ( 'NONE',  ( 13.00433657606611604, 139.2454419355441928, -9.442801289195550396 ) ) ;
#2380 = ORIENTED_EDGE ( 'NONE', *, *, #3707, .F. ) ;
#2381 = CARTESIAN_POINT ( 'NONE',  ( -31.89848094669885725, 100.0271397714182342, -5.500000000000000000 ) ) ;
#2382 = DIRECTION ( 'NONE',  ( 0.000000000000000000, 0.000000000000000000, -1.000000000000000000 ) ) ;
#2383 = DIRECTION ( 'NONE',  ( 0.000000000000000000, 0.000000000000000000, 1.000000000000000000 ) ) ;
#2384 = CARTESIAN_POINT ( 'NONE',  ( 34.53584570369260831, 194.4969340293141045, 23.78882387388086173 ) ) ;
#2385 = ADVANCED_FACE ( 'NONE', ( #4872, #7522 ), #546, .T. ) ;
#2386 = LINE ( 'NONE', #15855, #5557 ) ;
#2387 = AXIS2_PLACEMENT_3D ( 'NONE', #8252, #1524, #6920 ) ;
#2388 = LINE ( 'NONE', #7782, #12021 ) ;
#2389 = CYLINDRICAL_SURFACE ( 'NONE', #1670, 2.000000000000001776 ) ;
#2390 = AXIS2_PLACEMENT_3D ( 'NONE', #13418, #6695, #12090 ) ;
#2391 = CARTESIAN_POINT ( 'NONE',  ( 27.48361012698979877, 126.6227766016837819, 9.278408830390956550E-15 ) ) ;
#2392 = CARTESIAN_POINT ( 'NONE',  ( 34.78805733343664741, 142.9896906294144969, -20.13387259562453480 ) ) ;
#2393 = ORIENTED_EDGE ( 'NONE', *, *, #14927, .F. ) ;
#2394 = DIRECTION ( 'NONE',  ( -1.000000000000000000, 0.000000000000000000, 0.000000000000000000 ) ) ;
#2395 = VERTEX_POINT ( 'NONE', #14002 ) ;
#2396 = ADVANCED_FACE ( 'NONE', ( #12669 ), #3284, .T. ) ;
#2397 = LINE ( 'NONE', #2137, #12148 ) ;
#2398 = EDGE_CURVE ( 'NONE', #8931, #12797, #14184, .T. ) ;
#2399 = CARTESIAN_POINT ( 'NONE',  ( -68.00000000000000000, 171.6227766016838245, 19.49999999999998934 ) ) ;
#2400 = EDGE_LOOP ( 'NONE', ( #9524, #14647 ) ) ;
#2401 = CARTESIAN_POINT ( 'NONE',  ( -7.379000772444995526, 20.00000000000000355, 15.00000000000000178 ) ) ;
#2402 = CARTESIAN_POINT ( 'NONE',  ( 11.61604111307750209, 130.6582085322020532, 11.34316963496758390 ) ) ;
#2403 = CIRCLE ( 'NONE', #6661, 2.500000000000002220 ) ;
#2404 = ORIENTED_EDGE ( 'NONE', *, *, #2, .F. ) ;
#2405 = PRESENTATION_LAYER_ASSIGNMENT (  '', '', ( #14006 ) ) ;
#2406 = DIRECTION ( 'NONE',  ( 0.000000000000000000, 0.000000000000000000, -1.000000000000000000 ) ) ;
#2407 = AXIS2_PLACEMENT_3D ( 'NONE', #7831, #3428, #8894 ) ;
#2408 = ORIENTED_EDGE ( 'NONE', *, *, #13777, .T. ) ;
#2409 = DIRECTION ( 'NONE',  ( 0.000000000000000000, 0.000000000000000000, -1.000000000000000000 ) ) ;
#2410 = CARTESIAN_POINT ( 'NONE',  ( 48.00000000000000711, 183.6227766016837961, -3.071800142134975431 ) ) ;
#2411 = CARTESIAN_POINT ( 'NONE',  ( -17.03105419742079363, 32.06459626301238330, -9.633022903854756791 ) ) ;
#2412 = CARTESIAN_POINT ( 'NONE',  ( -12.73428483635692210, 18.00000000000460787, -6.504128904294631752 ) ) ;
#2413 = STYLED_ITEM ( 'NONE', ( #10047 ), #5407 ) ;
#2414 = VERTEX_POINT ( 'NONE', #4953 ) ;
#2415 = DIRECTION ( 'NONE',  ( 0.1091791256177803288, -0.4970110457850271390, -0.8608483832226269117 ) ) ;
#2416 =( GEOMETRIC_REPRESENTATION_CONTEXT ( 3 ) GLOBAL_UNCERTAINTY_ASSIGNED_CONTEXT ( ( #11805 ) ) GLOBAL_UNIT_ASSIGNED_CONTEXT ( ( #777, #6172, #686 ) ) REPRESENTATION_CONTEXT ( 'NONE', 'WORKASPACE' ) );
#2417 = EDGE_LOOP ( 'NONE', ( #3578, #120, #11351, #6584 ) ) ;
#2418 = CARTESIAN_POINT ( 'NONE',  ( 34.02269566797333056, 192.1516832787069404, -28.34894355864044613 ) ) ;
#2419 = DIRECTION ( 'NONE',  ( 0.000000000000000000, 0.000000000000000000, -1.000000000000000000 ) ) ;
#2420 = ORIENTED_EDGE ( 'NONE', *, *, #4150, .T. ) ;
#2421 = ORIENTED_EDGE ( 'NONE', *, *, #7525, .T. ) ;
#2422 = ORIENTED_EDGE ( 'NONE', *, *, #1329, .F. ) ;
#2423 = CARTESIAN_POINT ( 'NONE',  ( -73.65095110843941484, 150.6223998522366401, -25.45681811525069804 ) ) ;
#2424 = UNCERTAINTY_MEASURE_WITH_UNIT (LENGTH_MEASURE( 1.000000000000000082E-05 ), #9338, 'distance_accuracy_value', 'NONE');
#2425 = AXIS2_PLACEMENT_3D ( 'NONE', #2873, #8268, #13676 ) ;
#2426 = ORIENTED_EDGE ( 'NONE', *, *, #671, .T. ) ;
#2427 = EDGE_CURVE ( 'NONE', #12997, #13658, #4816, .T. ) ;
#2428 = CARTESIAN_POINT ( 'NONE',  ( 13.66341101666136382, 138.6227766017534293, -1.153153160029659841 ) ) ;
#2429 = CIRCLE ( 'NONE', #8090, 5.000000000000000888 ) ;
#2430 = CARTESIAN_POINT ( 'NONE',  ( -12.61248932541308676, 31.15232071419451643, 13.80069170922183375 ) ) ;
#2431 = CARTESIAN_POINT ( 'NONE',  ( 30.20986408795699418, 152.6234490708242220, -29.39431159376453095 ) ) ;
#2432 = CARTESIAN_POINT ( 'NONE',  ( 21.38389869590487891, 18.00000000000114753, 9.948751090973035005 ) ) ;
#2433 = CIRCLE ( 'NONE', #6680, 19.49999999999999645 ) ;
#2434 = CARTESIAN_POINT ( 'NONE',  ( -84.64785531711687838, 148.4718376841440204, 23.51742847763245337 ) ) ;
#2435 = ORIENTED_EDGE ( 'NONE', *, *, #12533, .F. ) ;
#2436 = CARTESIAN_POINT ( 'NONE',  ( 17.57170338634705331, 142.7189882356449857, 15.92841986281182187 ) ) ;
#2437 = CARTESIAN_POINT ( 'NONE',  ( -44.99999999999998579, 8.000000000000010658, 40.00000000000000000 ) ) ;
#2438 = CARTESIAN_POINT ( 'NONE',  ( 17.00000000000000000, 204.6227766016838245, -2.020667218593133100E-15 ) ) ;
#2439 = CARTESIAN_POINT ( 'NONE',  ( 32.91012024024373517, 17.99999999999999645, 13.86436652238006673 ) ) ;
#2440 = LINE ( 'NONE', #2353, #8732 ) ;
#2441 = VERTEX_POINT ( 'NONE', #16830 ) ;
#2442 = CARTESIAN_POINT ( 'NONE',  ( 2.426025403784448642, 0.000000000000000000, 0.000000000000000000 ) ) ;
#2443 = CIRCLE ( 'NONE', #14599, 7.500000000000000000 ) ;
#2444 = VECTOR ( 'NONE', #4957, 1000.000000000000000 ) ;
#2445 = CIRCLE ( 'NONE', #16307, 5.000000000000000888 ) ;
#2446 = CIRCLE ( 'NONE', #14895, 27.69059892324149530 ) ;
#2447 = CARTESIAN_POINT ( 'NONE',  ( 32.94631475844272472, 200.6745000914694117, 15.65774685523815890 ) ) ;
#2448 = ORIENTED_EDGE ( 'NONE', *, *, #13761, .F. ) ;
#2449 = FILL_AREA_STYLE ('',( #6435 ) ) ;
#2450 = CYLINDRICAL_SURFACE ( 'NONE', #12720, 24.99999999999999645 ) ;
#2451 = ORIENTED_EDGE ( 'NONE', *, *, #1601, .T. ) ;
#2452 = EDGE_CURVE ( 'NONE', #9465, #8476, #4703, .T. ) ;
#2453 = SURFACE_STYLE_USAGE ( .BOTH. , #10588 ) ;
#2454 = EDGE_CURVE ( 'NONE', #14218, #3754, #13004, .T. ) ;
#2455 = CARTESIAN_POINT ( 'NONE',  ( -24.99999999999999289, 100.0000000000000142, 15.00000000000000000 ) ) ;
#2456 = ADVANCED_FACE ( 'NONE', ( #717, #6114 ), #11511, .F. ) ;
#2457 = CIRCLE ( 'NONE', #1614, 5.315148208181398104 ) ;
#2458 = CARTESIAN_POINT ( 'NONE',  ( 20.11141720500412333, 18.00000000000000000, -24.32074799214299077 ) ) ;
#2459 = CARTESIAN_POINT ( 'NONE',  ( -74.00000000000002842, 146.6227766016838245, -24.49489742783179125 ) ) ;
#2460 = AXIS2_PLACEMENT_3D ( 'NONE', #8576, #7506, #8495 ) ;
#2461 = STYLED_ITEM ( 'NONE', ( #16877 ), #1721 ) ;
#2462 = CARTESIAN_POINT ( 'NONE',  ( -27.81025873171733664, 19.99999999999999289, 7.666431193274479305 ) ) ;
#2463 = COLOUR_RGB ( '', 0.72549020, 0.75294118, 0.79215686) ;
#2464 = ORIENTED_EDGE ( 'NONE', *, *, #13937, .F. ) ;
#2465 = CARTESIAN_POINT ( 'NONE',  ( 27.48361012698979522, 126.6227766016837819, 6.072704737864100906E-13 ) ) ;
#2466 = CARTESIAN_POINT ( 'NONE',  ( 12.11856678106299512, 143.7750213247282431, 17.70723251555758537 ) ) ;
#2467 = PLANE ( 'NONE',  #11306 ) ;
#2468 = CARTESIAN_POINT ( 'NONE',  ( 35.74205400282647815, 198.3976433773784152, -22.54711430683565254 ) ) ;
#2469 = ORIENTED_EDGE ( 'NONE', *, *, #10090, .F. ) ;
#2470 = VERTEX_POINT ( 'NONE', #6364 ) ;
#2471 = CARTESIAN_POINT ( 'NONE',  ( 8.608950980928550933, 133.4921716645119432, -14.72901497434506091 ) ) ;
#2472 = AXIS2_PLACEMENT_3D ( 'NONE', #5028, #10419, #9274 ) ;
#2473 = ORIENTED_EDGE ( 'NONE', *, *, #2718, .F. ) ;
#2474 = CARTESIAN_POINT ( 'NONE',  ( -84.31958363394323897, 150.8057096996395785, -28.13880055569950400 ) ) ;
#2475 = CIRCLE ( 'NONE', #12661, 5.000000000000004441 ) ;
#2476 = CARTESIAN_POINT ( 'NONE',  ( 13.85534145189780197, 143.5014890223674229, -17.26861023069377410 ) ) ;
#2477 = VERTEX_POINT ( 'NONE', #15930 ) ;
#2478 = CARTESIAN_POINT ( 'NONE',  ( -27.99999999999998224, 10.00000000000000000, 10.00000000000000178 ) ) ;
#2479 = FACE_OUTER_BOUND ( 'NONE', #7297, .T. ) ;
#2480 = LINE ( 'NONE', #7877, #4714 ) ;
#2481 = FACE_OUTER_BOUND ( 'NONE', #13023, .T. ) ;
#2482 = CARTESIAN_POINT ( 'NONE',  ( 34.80444759354871564, 18.00000000000000000, -7.621511755358874929 ) ) ;
#2483 = DIRECTION ( 'NONE',  ( 1.000000000000000000, -1.243449787580175325E-14, 0.000000000000000000 ) ) ;
#2484 = CYLINDRICAL_SURFACE ( 'NONE', #17506, 2.500000000000000444 ) ;
#2485 = CARTESIAN_POINT ( 'NONE',  ( 225.0000000000000000, 89.99999999999997158, 15.00000000000000000 ) ) ;
#2486 = VECTOR ( 'NONE', #6462, 1000.000000000000000 ) ;
#2487 = PRESENTATION_LAYER_ASSIGNMENT (  '', '', ( #10112 ) ) ;
#2488 = DIRECTION ( 'NONE',  ( -1.000000000000000000, -0.000000000000000000, -0.000000000000000000 ) ) ;
#2489 = ORIENTED_EDGE ( 'NONE', *, *, #8581, .F. ) ;
#2490 = DIRECTION ( 'NONE',  ( 0.000000000000000000, -1.000000000000000000, 0.000000000000000000 ) ) ;
#2491 = CARTESIAN_POINT ( 'NONE',  ( -25.15885279626527193, 20.00000000000000355, -15.13659797665870776 ) ) ;
#2492 = ORIENTED_EDGE ( 'NONE', *, *, #1855, .F. ) ;
#2493 = CARTESIAN_POINT ( 'NONE',  ( 48.00000000000000711, 175.6227766016838530, 19.42820660268601074 ) ) ;
#2494 = B_SPLINE_CURVE_WITH_KNOTS ( 'NONE', 3,
 ( #6445, #17249, #7857, #10785, #13268, #9183, #9275, #3786, #15833, #5124, #15917, #16195, #1139, #5029 ),
 .UNSPECIFIED., .F., .F.,
 ( 4, 2, 2, 2, 2, 2, 4 ),
 ( 0.000000000000000000, 0.0006954478661160458245, 0.001043171799174067707, 0.001390895732232089697, 0.001738619665290111688, 0.002086343598348133679, 0.002781791464464176359 ),
 .UNSPECIFIED. ) ;
#2495 = CARTESIAN_POINT ( 'NONE',  ( -27.99999999999998224, 10.00000000000000000, 0.000000000000000000 ) ) ;
#2496 = ADVANCED_FACE ( 'NONE', ( #13189 ), #14781, .T. ) ;
#2497 = ORIENTED_EDGE ( 'NONE', *, *, #12512, .F. ) ;
#2498 = EDGE_CURVE ( 'NONE', #10657, #14819, #17440, .T. ) ;
#2499 = CARTESIAN_POINT ( 'NONE',  ( 13.23724818701972161, 139.1606502921264905, 9.139539437136063427 ) ) ;
#2500 = VERTEX_POINT ( 'NONE', #7964 ) ;
#2501 = CIRCLE ( 'NONE', #10408, 6.000000000000005329 ) ;
#2502 = CARTESIAN_POINT ( 'NONE',  ( 14.93242934743711814, 20.00000000000000355, 15.00000000000000000 ) ) ;
#2503 = VECTOR ( 'NONE', #5389, 1000.000000000000114 ) ;
#2504 = EDGE_LOOP ( 'NONE', ( #10553, #11632 ) ) ;
#2505 = DIRECTION ( 'NONE',  ( 0.000000000000000000, 0.000000000000000000, -1.000000000000000000 ) ) ;
#2506 = EDGE_CURVE ( 'NONE', #12384, #4864, #8481, .T. ) ;
#2507 = DIRECTION ( 'NONE',  ( 0.000000000000000000, 0.000000000000000000, 1.000000000000000000 ) ) ;
#2508 = DIRECTION ( 'NONE',  ( 0.000000000000000000, 0.000000000000000000, 1.000000000000000000 ) ) ;
#2509 = CARTESIAN_POINT ( 'NONE',  ( -13.91527097789399292, 18.00000000000000000, -23.98152295253420618 ) ) ;
#2510 = EDGE_LOOP ( 'NONE', ( #15619, #16735, #9470, #1525 ) ) ;
#2511 = CARTESIAN_POINT ( 'NONE',  ( 28.44374398009894023, 151.3901271056992925, 26.07015880384262729 ) ) ;
#2512 = VECTOR ( 'NONE', #14109, 1000.000000000000000 ) ;
#2513 = ORIENTED_EDGE ( 'NONE', *, *, #15448, .T. ) ;
#2514 = CARTESIAN_POINT ( 'NONE',  ( -207.6770884633516516, 175.2440045654562368, -3.971992828049704993 ) ) ;
#2515 = AXIS2_PLACEMENT_3D ( 'NONE', #9598, #4298, #16250 ) ;
#2516 = CARTESIAN_POINT ( 'NONE',  ( -87.50000000000005684, 197.1893936856112362, -20.88304578468306616 ) ) ;
#2517 = ORIENTED_EDGE ( 'NONE', *, *, #12004, .T. ) ;
#2518 = EDGE_LOOP ( 'NONE', ( #5778, #8527, #8409, #3295, #5549, #10328, #13109, #13182, #5802, #8393 ) ) ;
#2519 = EDGE_LOOP ( 'NONE', ( #17207, #12810, #15335, #13234 ) ) ;
#2520 = EDGE_CURVE ( 'NONE', #6066, #5020, #9110, .T. ) ;
#2521 = CARTESIAN_POINT ( 'NONE',  ( 196.0000000000000000, 179.6227766016838245, 10.00000337241049309 ) ) ;
#2522 = AXIS2_PLACEMENT_3D ( 'NONE', #5850, #6839, #2849 ) ;
#2523 = AXIS2_PLACEMENT_3D ( 'NONE', #6254, #15465, #11391 ) ;
#2524 = ADVANCED_FACE ( 'NONE', ( #13453 ), #14982, .F. ) ;
#2525 = ORIENTED_EDGE ( 'NONE', *, *, #3118, .T. ) ;
#2526 = DIRECTION ( 'NONE',  ( 0.000000000000000000, 0.000000000000000000, 1.000000000000000000 ) ) ;
#2527 = AXIS2_PLACEMENT_3D ( 'NONE', #906, #6294, #11684 ) ;
#2528 = FACE_OUTER_BOUND ( 'NONE', #2510, .T. ) ;
#2529 = EDGE_CURVE ( 'NONE', #12961, #8416, #16124, .T. ) ;
#2530 = CIRCLE ( 'NONE', #8469, 20.00000000000000355 ) ;
#2531 = CARTESIAN_POINT ( 'NONE',  ( -18.25212770525997286, 32.30769230769230660, 4.999999999999999112 ) ) ;
#2532 = EDGE_CURVE ( 'NONE', #12169, #6282, #17262, .T. ) ;
#2533 = DIRECTION ( 'NONE',  ( -1.000000000000000000, 0.000000000000000000, 0.000000000000000000 ) ) ;
#2534 = CARTESIAN_POINT ( 'NONE',  ( 48.00000000000000711, 183.6227766016837961, 5.571800142134975431 ) ) ;
#2535 = CARTESIAN_POINT ( 'NONE',  ( -80.40558230539225804, 151.6102025845144112, 26.23924109008941130 ) ) ;
#2536 = EDGE_LOOP ( 'NONE', ( #10221, #42, #10080 ) ) ;
#2537 = DIRECTION ( 'NONE',  ( 1.000000000000000000, 0.000000000000000000, -0.000000000000000000 ) ) ;
#2538 = DIRECTION ( 'NONE',  ( 0.000000000000000000, 0.000000000000000000, 1.000000000000000000 ) ) ;
#2539 = DIRECTION ( 'NONE',  ( -0.000000000000000000, -0.000000000000000000, 1.000000000000000000 ) ) ;
#2540 = DIRECTION ( 'NONE',  ( 0.000000000000000000, -8.673617379884035472E-17, -1.000000000000000000 ) ) ;
#2541 = DIRECTION ( 'NONE',  ( -1.000000000000000000, 0.000000000000000000, -8.673617379884037937E-17 ) ) ;
#2542 = ORIENTED_EDGE ( 'NONE', *, *, #197, .F. ) ;
#2543 = PLANE ( 'NONE',  #1576 ) ;
#2544 = VECTOR ( 'NONE', #16275, 1000.000000000000114 ) ;
#2545 = EDGE_CURVE ( 'NONE', #10551, #6443, #4251, .T. ) ;
#2546 = AXIS2_PLACEMENT_3D ( 'NONE', #282, #444, #5594 ) ;
#2547 = CARTESIAN_POINT ( 'NONE',  ( 28.84079492301047765, 201.4909985710883689, 14.03234625026787619 ) ) ;
#2548 = VERTEX_POINT ( 'NONE', #14438 ) ;
#2549 = LINE ( 'NONE', #871, #15753 ) ;
#2550 = CARTESIAN_POINT ( 'NONE',  ( -40.00000000000000000, 4.000000000000000000, -33.00000000000000711 ) ) ;
#2551 = EDGE_LOOP ( 'NONE', ( #10113, #15537, #14761, #2542 ) ) ;
#2552 =( NAMED_UNIT ( * ) PLANE_ANGLE_UNIT ( ) SI_UNIT ( $, .RADIAN. ) );
#2553 = CARTESIAN_POINT ( 'NONE',  ( -75.02794788578133023, 146.0169975363980370, 20.82225907110315788 ) ) ;
#2554 = CARTESIAN_POINT ( 'NONE',  ( 15.00000000000000000, 143.0344144757318929, -16.50549856913627877 ) ) ;
#2555 = AXIS2_PLACEMENT_3D ( 'NONE', #4671, #1838, #11481 ) ;
#2556 = CARTESIAN_POINT ( 'NONE',  ( -74.00000000000002842, 145.8714137932802544, -23.72804097270956802 ) ) ;
#2557 = CIRCLE ( 'NONE', #16121, 19.49999999999998934 ) ;
#2558 = AXIS2_PLACEMENT_3D ( 'NONE', #1304, #5022, #1213 ) ;
#2559 = CARTESIAN_POINT ( 'NONE',  ( -16.40540729975244005, 20.00000000000000000, 23.03124090058168960 ) ) ;
#2560 = ORIENTED_EDGE ( 'NONE', *, *, #12281, .T. ) ;
#2561 = CARTESIAN_POINT ( 'NONE',  ( 40.00000000000000711, 171.6227766016838245, 0.000000000000000000 ) ) ;
#2562 = DIRECTION ( 'NONE',  ( 0.000000000000000000, 1.000000000000000000, 0.000000000000000000 ) ) ;
#2563 = CARTESIAN_POINT ( 'NONE',  ( -208.0000000000000853, 123.4836845632602262, -24.20219073603711735 ) ) ;
#2564 = DIRECTION ( 'NONE',  ( -0.7071067811865513475, 0.000000000000000000, 0.7071067811865436870 ) ) ;
#2565 = EDGE_CURVE ( 'NONE', #14379, #1461, #573, .T. ) ;
#2566 = EDGE_CURVE ( 'NONE', #6747, #5655, #4534, .T. ) ;
#2567 = ADVANCED_FACE ( 'NONE', ( #1235 ), #12129, .F. ) ;
#2568 = ORIENTED_EDGE ( 'NONE', *, *, #1094, .F. ) ;
#2569 = ADVANCED_BREP_SHAPE_REPRESENTATION ( '', ( #5314, #3583 ), #803 ) ;
#2570 = AXIS2_PLACEMENT_3D ( 'NONE', #6870, #9425, #13248 ) ;
#2571 = CARTESIAN_POINT ( 'NONE',  ( 9.380362127004868711, 139.2112497869900949, -14.33999639901018242 ) ) ;
#2572 = VERTEX_POINT ( 'NONE', #11945 ) ;
#2573 = CARTESIAN_POINT ( 'NONE',  ( -84.03010877036541615, 151.0873486859324828, -28.34424093584476623 ) ) ;
#2574 = CIRCLE ( 'NONE', #2004, 7.500000000000000000 ) ;
#2575 = CARTESIAN_POINT ( 'NONE',  ( 24.34257225596280350, 140.5456842492515932, -11.13195485280035513 ) ) ;
#2576 = ORIENTED_EDGE ( 'NONE', *, *, #17330, .F. ) ;
#2577 = LINE ( 'NONE', #14514, #5309 ) ;
#2578 = DIRECTION ( 'NONE',  ( -0.000000000000000000, -0.000000000000000000, -1.000000000000000000 ) ) ;
#2579 = DIRECTION ( 'NONE',  ( -1.000000000000000000, 0.000000000000000000, 0.000000000000000000 ) ) ;
#2580 = APPLICATION_CONTEXT ( 'automotive_design' ) ;
#2581 = DIRECTION ( 'NONE',  ( -1.000000000000000000, 0.000000000000000000, 0.000000000000000000 ) ) ;
#2582 = DIRECTION ( 'NONE',  ( 0.000000000000000000, -1.000000000000000000, 0.000000000000000000 ) ) ;
#2583 = CARTESIAN_POINT ( 'NONE',  ( 21.36708699129047773, 18.00000000000000000, -23.94811280430834088 ) ) ;
#2584 = LINE ( 'NONE', #14786, #11225 ) ;
#2585 = DIRECTION ( 'NONE',  ( 0.000000000000000000, 1.000000000000000000, 0.000000000000000000 ) ) ;
#2586 = CARTESIAN_POINT ( 'NONE',  ( 196.0000000000000000, 171.6227766016838245, 12.50000337241049131 ) ) ;
#2587 = FACE_OUTER_BOUND ( 'NONE', #180, .T. ) ;
#2588 = ORIENTED_EDGE ( 'NONE', *, *, #6679, .F. ) ;
#2589 = FACE_OUTER_BOUND ( 'NONE', #7027, .T. ) ;
#2590 = EDGE_CURVE ( 'NONE', #4871, #8198, #7069, .T. ) ;
#2591 = ORIENTED_EDGE ( 'NONE', *, *, #78, .F. ) ;
#2592 = DIRECTION ( 'NONE',  ( 0.000000000000000000, 1.000000000000000000, 0.000000000000000000 ) ) ;
#2593 = DIRECTION ( 'NONE',  ( 1.000000000000000000, 0.000000000000000000, -0.000000000000000000 ) ) ;
#2594 = ORIENTED_EDGE ( 'NONE', *, *, #4717, .T. ) ;
#2595 = CARTESIAN_POINT ( 'NONE',  ( -11.99122994684825549, 19.99999999999999645, 24.50500383881168176 ) ) ;
#2596 = CARTESIAN_POINT ( 'NONE',  ( 23.14977753070779087, 141.0007991078602743, 12.30735618844933832 ) ) ;
#2597 = AXIS2_PLACEMENT_3D ( 'NONE', #16693, #14032, #1898 ) ;
#2598 = ORIENTED_EDGE ( 'NONE', *, *, #9370, .F. ) ;
#2599 = CARTESIAN_POINT ( 'NONE',  ( -725.0000000000000000, 30.00000000000000000, -13.00000000000000000 ) ) ;
#2600 = ORIENTED_EDGE ( 'NONE', *, *, #3605, .T. ) ;
#2601 = CARTESIAN_POINT ( 'NONE',  ( 15.00000000000000000, 154.3022685259950038, 9.999999999999900524 ) ) ;
#2602 = DIRECTION ( 'NONE',  ( 1.000000000000000000, -0.000000000000000000, -0.000000000000000000 ) ) ;
#2603 = DIRECTION ( 'NONE',  ( -0.000000000000000000, -1.000000000000000000, -0.000000000000000000 ) ) ;
#2604 = CARTESIAN_POINT ( 'NONE',  ( -11.94789857657465681, 18.00000000000115108, -9.192893430571174918 ) ) ;
#2605 = ADVANCED_FACE ( 'NONE', ( #9197 ), #10613, .F. ) ;
#2606 = VERTEX_POINT ( 'NONE', #4000 ) ;
#2607 = CARTESIAN_POINT ( 'NONE',  ( 25.75259266847351469, 149.2783667126899445, 24.28707720053400720 ) ) ;
#2608 = ORIENTED_EDGE ( 'NONE', *, *, #6258, .T. ) ;
#2609 = CARTESIAN_POINT ( 'NONE',  ( -73.19504936680527862, 193.4351830419512623, -24.76910924193871466 ) ) ;
#2610 = DIRECTION ( 'NONE',  ( -0.000000000000000000, -0.000000000000000000, -1.000000000000000000 ) ) ;
#2611 =( BOUNDED_SURFACE ( )  B_SPLINE_SURFACE ( 3, 2, ( 
 ( #9823, #16659, #4528 ),
 ( #9914, #7003, #355 ),
 ( #4611, #16399, #3104 ),
 ( #9646, #9989, #12399 ),
 ( #7170, #537, #12570 ),
 ( #436, #11337, #15398 ),
 ( #4265, #271, #5842 ),
 ( #5677, #12660, #8677 ),
 ( #1861, #14087, #15317 ),
 ( #16480, #3190, #7258 ),
 ( #15129, #5942, #3276 ),
 ( #1949, #889, #15489 ),
 ( #15579, #8843, #13014 ),
 ( #4945, #11411, #3455 ),
 ( #14334, #7432, #3370 ),
 ( #16910, #4866, #14251 ),
 ( #14177, #4785, #711 ),
 ( #3537, #12833, #6104 ),
 ( #9017, #2115, #10175 ),
 ( #7513, #10083, #11502 ),
 ( #14429, #12923, #16823 ),
 ( #801, #7603, #6192 ),
 ( #11592, #2038, #7687 ),
 ( #11667, #17000, #2204 ),
 ( #10256, #15655, #8925 ),
 ( #6277, #17075, #10339 ),
 ( #15747, #3625, #2295 ),
 ( #8764, #13095, #960 ) ),
 .UNSPECIFIED., .F., .F., .F. ) 
 B_SPLINE_SURFACE_WITH_KNOTS ( ( 4, 2, 2, 2, 2, 2, 2, 2, 2, 2, 2, 2, 2, 4 ),
 ( 3, 3 ),
 ( 0.01342997177288654184, 0.01733910390705691029, 0.01929366997414209278, 0.02124823604122727527, 0.02515736817539764372, 0.02711193424248282968, 0.02906650030956801217, 0.03297563244373838409, 0.03493019851082356658, 0.03688476457790874907, 0.03883933064499393156, 0.03981661367853651934, 0.04079389671207911405, 0.04470302884624948597 ),
 ( 0.000000000000000000, 1.000000000000000000 ),
 .UNSPECIFIED. ) 
 GEOMETRIC_REPRESENTATION_ITEM ( )  RATIONAL_B_SPLINE_SURFACE ( (
 ( 1.000000000000000000, 0.7117435966472906994, 1.000000000000000000),
 ( 1.000000000000000000, 0.7117434842622788471, 1.000000000000000000),
 ( 1.000000000000000000, 0.7117144184576317256, 1.000000000000000000),
 ( 1.000000000000000000, 0.7116285301813536357, 1.000000000000000000),
 ( 1.000000000000000000, 0.7115928256594988843, 1.000000000000000000),
 ( 1.000000000000000000, 0.7115068832447583036, 1.000000000000000000),
 ( 1.000000000000000000, 0.7114564033771691998, 1.000000000000000000),
 ( 1.000000000000000000, 0.7112861117250206533, 1.000000000000000000),
 ( 1.000000000000000000, 0.7111469280185451769, 1.000000000000000000),
 ( 1.000000000000000000, 0.7108993804763810154, 1.000000000000000000),
 ( 1.000000000000000000, 0.7108100171490498997, 1.000000000000000000),
 ( 1.000000000000000000, 0.7106191415567917335, 1.000000000000000000),
 ( 1.000000000000000000, 0.7105185320923617098, 1.000000000000000000),
 ( 1.000000000000000000, 0.7102014790723296667, 1.000000000000000000),
 ( 1.000000000000000000, 0.7099699576741209661, 1.000000000000000000),
 ( 1.000000000000000000, 0.7095909300314675594, 1.000000000000000000),
 ( 1.000000000000000000, 0.7094593121158619953, 1.000000000000000000),
 ( 1.000000000000000000, 0.7091910831478104305, 1.000000000000000000),
 ( 1.000000000000000000, 0.7090537746377190143, 1.000000000000000000),
 ( 1.000000000000000000, 0.7087727591781516345, 1.000000000000000000),
 ( 1.000000000000000000, 0.7086290523620303317, 1.000000000000000000),
 ( 1.000000000000000000, 0.7084085592173990920, 1.000000000000000000),
 ( 1.000000000000000000, 0.7083342380282030559, 1.000000000000000000),
 ( 1.000000000000000000, 0.7081839094108949295, 1.000000000000000000),
 ( 1.000000000000000000, 0.7081077478408516201, 1.000000000000000000),
 ( 1.000000000000000000, 0.7077267031859736379, 1.000000000000000000),
 ( 1.000000000000000000, 0.7074184602292508117, 1.000000000000000000),
 ( 1.000000000000000000, 0.7071067811865475727, 1.000000000000000000) ) ) 
 REPRESENTATION_ITEM ( '' )  SURFACE ( )  );
#2612 = ORIENTED_EDGE ( 'NONE', *, *, #337, .F. ) ;
#2613 = ORIENTED_EDGE ( 'NONE', *, *, #10834, .T. ) ;
#2614 = EDGE_LOOP ( 'NONE', ( #6751, #6307, #16661, #2906 ) ) ;
#2615 = FACE_OUTER_BOUND ( 'NONE', #17467, .T. ) ;
#2616 = VERTEX_POINT ( 'NONE', #5044 ) ;
#2617 = DIRECTION ( 'NONE',  ( -1.000000000000000000, 0.000000000000000000, 0.000000000000000000 ) ) ;
#2618 = DIRECTION ( 'NONE',  ( -1.000000000000000000, 0.000000000000000000, 0.000000000000000000 ) ) ;
#2619 = CARTESIAN_POINT ( 'NONE',  ( 36.00000000000002132, 146.6227766016838245, -24.49489742783179125 ) ) ;
#2620 = CYLINDRICAL_SURFACE ( 'NONE', #40, 4.750000000000000000 ) ;
#2621 = CARTESIAN_POINT ( 'NONE',  ( -83.66276280984922664, 150.0417915422717385, 24.96744664354709897 ) ) ;
#2622 = EDGE_CURVE ( 'NONE', #5481, #16728, #12437, .T. ) ;
#2623 = VERTEX_POINT ( 'NONE', #9287 ) ;
#2624 = CARTESIAN_POINT ( 'NONE',  ( -85.34459197722598844, 199.3716779298525807, -21.33657927093678808 ) ) ;
#2625 = CARTESIAN_POINT ( 'NONE',  ( 18.16062352778163813, 29.95676120085481386, -14.47054584901207619 ) ) ;
#2626 = CARTESIAN_POINT ( 'NONE',  ( -50.00000000000000000, 171.6227766016838245, -2.602085213965210642E-15 ) ) ;
#2627 = DIRECTION ( 'NONE',  ( 1.000000000000000000, -0.000000000000000000, -0.000000000000000000 ) ) ;
#2628 = CYLINDRICAL_SURFACE ( 'NONE', #16666, 20.00000000000000355 ) ;
#2629 = ORIENTED_EDGE ( 'NONE', *, *, #12849, .F. ) ;
#2630 = CARTESIAN_POINT ( 'NONE',  ( -87.21337428997478014, 144.5042670319084550, -18.82352572523458889 ) ) ;
#2631 = EDGE_CURVE ( 'NONE', #8768, #6671, #15852, .T. ) ;
#2632 = EDGE_CURVE ( 'NONE', #7206, #9188, #16191, .T. ) ;
#2633 = FACE_OUTER_BOUND ( 'NONE', #2614, .T. ) ;
#2634 = LINE ( 'NONE', #4132, #9607 ) ;
#2635 = ORIENTED_EDGE ( 'NONE', *, *, #4081, .T. ) ;
#2636 = DIRECTION ( 'NONE',  ( 0.000000000000000000, 0.000000000000000000, 1.000000000000000000 ) ) ;
#2637 = VERTEX_POINT ( 'NONE', #5483 ) ;
#2638 = CARTESIAN_POINT ( 'NONE',  ( 39.99999999999998579, 4.000000000000000000, -33.00000000000000711 ) ) ;
#2639 = DIRECTION ( 'NONE',  ( 1.000000000000000000, 0.000000000000000000, 0.000000000000000000 ) ) ;
#2640 = CARTESIAN_POINT ( 'NONE',  ( -81.04928679900669408, 140.7094120356993585, -16.41247553121493752 ) ) ;
#2641 = DIRECTION ( 'NONE',  ( 0.000000000000000000, 0.000000000000000000, 1.000000000000000000 ) ) ;
#2642 = EDGE_LOOP ( 'NONE', ( #17068, #9628, #2768, #7721 ) ) ;
#2643 = DIRECTION ( 'NONE',  ( 0.000000000000000000, 0.000000000000000000, 1.000000000000000000 ) ) ;
#2644 = CARTESIAN_POINT ( 'NONE',  ( -23.00000000000000000, 120.0000000000000426, 15.00000000000000000 ) ) ;
#2645 = DIRECTION ( 'NONE',  ( 0.000000000000000000, 0.000000000000000000, -1.000000000000000000 ) ) ;
#2646 = LINE ( 'NONE', #14593, #6086 ) ;
#2647 = EDGE_LOOP ( 'NONE', ( #41, #6678, #14964 ) ) ;
#2648 = CARTESIAN_POINT ( 'NONE',  ( 22.72753210816244618, 139.3086630800672765, -13.45249220522710232 ) ) ;
#2649 = ORIENTED_EDGE ( 'NONE', *, *, #16804, .F. ) ;
#2650 = CARTESIAN_POINT ( 'NONE',  ( -79.79013591204304134, 152.6234490708242504, -29.39431159376453806 ) ) ;
#2651 = CARTESIAN_POINT ( 'NONE',  ( 26.57417986947462651, 139.5089559931849692, -7.600184560211070917 ) ) ;
#2652 = ORIENTED_EDGE ( 'NONE', *, *, #10245, .T. ) ;
#2653 = CARTESIAN_POINT ( 'NONE',  ( -3.000000000000000888, 171.6227766016838245, 0.000000000000000000 ) ) ;
#2654 = DIRECTION ( 'NONE',  ( 1.000000000000000000, 0.000000000000000000, -0.000000000000000000 ) ) ;
#2655 = DIRECTION ( 'NONE',  ( -0.08715574274764661955, -0.4980973490458647235, -0.8627299156628267518 ) ) ;
#2656 = ADVANCED_FACE ( 'NONE', ( #13544 ), #9718, .T. ) ;
#2657 = DIRECTION ( 'NONE',  ( -0.000000000000000000, -0.000000000000000000, 1.000000000000000000 ) ) ;
#2658 = CARTESIAN_POINT ( 'NONE',  ( 21.38845554303141938, 18.00000000000000000, -23.94082098111162082 ) ) ;
#2659 = CARTESIAN_POINT ( 'NONE',  ( 19.81659905433974700, 29.90262535319825332, -11.35915249282563444 ) ) ;
#2660 = LINE ( 'NONE', #171, #7546 ) ;
#2661 = LINE ( 'NONE', #7970, #10421 ) ;
#2662 = DIRECTION ( 'NONE',  ( 7.523163845262643335E-32, 1.000000000000000000, -8.673617379884037444E-16 ) ) ;
#2663 = PRESENTATION_STYLE_ASSIGNMENT (( #7884 ) ) ;
#2664 = CIRCLE ( 'NONE', #10279, 2.500000000000002220 ) ;
#2665 = VERTEX_POINT ( 'NONE', #16469 ) ;
#2666 = DIRECTION ( 'NONE',  ( 0.9961946980917461003, -0.04357787137382628656, 0.07547908730516766918 ) ) ;
#2667 = ORIENTED_EDGE ( 'NONE', *, *, #8607, .F. ) ;
#2668 = CARTESIAN_POINT ( 'NONE',  ( -71.66708739526794147, 110.0000000000000142, 4.500000000000000000 ) ) ;
#2669 = LINE ( 'NONE', #1249, #1321 ) ;
#2670 = EDGE_LOOP ( 'NONE', ( #5847, #14722, #17390, #10744, #8749 ) ) ;
#2671 = CYLINDRICAL_SURFACE ( 'NONE', #122, 5.000000000000000888 ) ;
#2672 = CARTESIAN_POINT ( 'NONE',  ( 15.54198151645489645, 125.3641151175237667, 5.547502007357641318 ) ) ;
#2673 = ORIENTED_EDGE ( 'NONE', *, *, #15766, .T. ) ;
#2674 = DIRECTION ( 'NONE',  ( 1.000000000000000000, 0.000000000000000000, 0.000000000000000000 ) ) ;
#2675 = AXIS2_PLACEMENT_3D ( 'NONE', #8938, #9298, #10533 ) ;
#2676 = ORIENTED_EDGE ( 'NONE', *, *, #10954, .T. ) ;
#2677 = ADVANCED_FACE ( 'NONE', ( #12557 ), #1420, .F. ) ;
#2678 = EDGE_CURVE ( 'NONE', #14137, #7753, #1985, .T. ) ;
#2679 = VECTOR ( 'NONE', #4455, 1000.000000000000000 ) ;
#2680 = EDGE_CURVE ( 'NONE', #14929, #9167, #6822, .T. ) ;
#2681 = EDGE_CURVE ( 'NONE', #1652, #10063, #3968, .T. ) ;
#2682 = DIRECTION ( 'NONE',  ( 0.000000000000000000, 0.000000000000000000, -1.000000000000000000 ) ) ;
#2683 = CARTESIAN_POINT ( 'NONE',  ( 37.50000000000001421, 196.4352734575233228, -21.75827460206395614 ) ) ;
#2684 = CARTESIAN_POINT ( 'NONE',  ( 17.58250999373992585, 125.2198453306090329, 1.325401613797208934E-14 ) ) ;
#2685 = DIRECTION ( 'NONE',  ( 1.000000000000000000, 0.000000000000000000, 0.000000000000000000 ) ) ;
#2686 = ORIENTED_EDGE ( 'NONE', *, *, #9891, .F. ) ;
#2687 = CARTESIAN_POINT ( 'NONE',  ( 33.41665845754520348, 150.2902214191208259, 25.17945278758671890 ) ) ;
#2688 = ORIENTED_EDGE ( 'NONE', *, *, #5475, .F. ) ;
#2689 = CARTESIAN_POINT ( 'NONE',  ( 32.50000000000000000, 196.6227766016838245, -16.00000000000000000 ) ) ;
#2690 = CARTESIAN_POINT ( 'NONE',  ( -50.00000000000000000, 171.6227766016838245, -19.49999999999998934 ) ) ;
#2691 = VECTOR ( 'NONE', #11767, 1000.000000000000000 ) ;
#2692 = ORIENTED_EDGE ( 'NONE', *, *, #3359, .F. ) ;
#2693 = CIRCLE ( 'NONE', #1551, 33.00000000000000000 ) ;
#2694 = ORIENTED_EDGE ( 'NONE', *, *, #13429, .T. ) ;
#2695 = ORIENTED_EDGE ( 'NONE', *, *, #4283, .F. ) ;
#2696 = EDGE_CURVE ( 'NONE', #2293, #8849, #17025, .T. ) ;
#2697 = CARTESIAN_POINT ( 'NONE',  ( -30.49999999999998224, 10.00000000000000000, 10.00000000000000178 ) ) ;
#2698 = ORIENTED_EDGE ( 'NONE', *, *, #10082, .T. ) ;
#2699 = DIRECTION ( 'NONE',  ( 0.000000000000000000, 0.000000000000000000, 1.000000000000000000 ) ) ;
#2700 = CARTESIAN_POINT ( 'NONE',  ( 17.00000000000000000, 171.6227766016838245, 0.000000000000000000 ) ) ;
#2701 = DIRECTION ( 'NONE',  ( 0.000000000000000000, -1.000000000000000000, 0.000000000000000000 ) ) ;
#2702 = CIRCLE ( 'NONE', #4118, 27.69059892324149530 ) ;
#2703 = CARTESIAN_POINT ( 'NONE',  ( -100.0000000000000000, 136.6227766016838245, 0.000000000000000000 ) ) ;
#2704 = DIRECTION ( 'NONE',  ( 0.000000000000000000, 0.000000000000000000, -1.000000000000000000 ) ) ;
#2705 = CARTESIAN_POINT ( 'NONE',  ( -100.0000000000000000, 171.6227766016838245, 0.000000000000000000 ) ) ;
#2706 = COLOUR_RGB ( '', 0.09019608, 0.27058824, 0.51372549) ;
#2707 = CIRCLE ( 'NONE', #12597, 19.49999999999998934 ) ;
#2708 = EDGE_LOOP ( 'NONE', ( #3084, #10998, #13647, #592, #17481 ) ) ;
#2709 = CARTESIAN_POINT ( 'NONE',  ( -81.97708560105468223, 202.2921397697441535, -16.86471387523356213 ) ) ;
#2710 = CARTESIAN_POINT ( 'NONE',  ( 36.00000000000002132, 146.6227766016838245, -35.00000000000000000 ) ) ;
#2711 = CARTESIAN_POINT ( 'NONE',  ( 21.38845554303141938, 18.00000000000000000, 23.94082098111162082 ) ) ;
#2712 = FACE_OUTER_BOUND ( 'NONE', #6902, .T. ) ;
#2713 = CARTESIAN_POINT ( 'NONE',  ( -48.00000000000000000, 171.6227766016838245, 0.000000000000000000 ) ) ;
#2714 = CIRCLE ( 'NONE', #8655, 2.500000000000002220 ) ;
#2715 = DIRECTION ( 'NONE',  ( 1.000000000000000000, 0.000000000000000000, 0.000000000000000000 ) ) ;
#2716 = EDGE_CURVE ( 'NONE', #2293, #11521, #11401, .T. ) ;
#2717 = VERTEX_POINT ( 'NONE', #6180 ) ;
#2718 = EDGE_CURVE ( 'NONE', #12692, #5700, #12173, .T. ) ;
#2719 = LINE ( 'NONE', #1482, #12080 ) ;
#2720 = ORIENTED_EDGE ( 'NONE', *, *, #2073, .T. ) ;
#2721 =( NAMED_UNIT ( * ) SI_UNIT ( $, .STERADIAN. ) SOLID_ANGLE_UNIT ( ) );
#2722 = LINE ( 'NONE', #3240, #17258 ) ;
#2723 = CARTESIAN_POINT ( 'NONE',  ( 27.99999999999998224, 9.999999999999998224, -28.00000000000001066 ) ) ;
#2724 = CARTESIAN_POINT ( 'NONE',  ( 22.99999999999997868, 9.999999999999998224, -12.99999999999999822 ) ) ;
#2725 = CARTESIAN_POINT ( 'NONE',  ( -20.85266279178580362, 19.99999999999999645, 20.15433268689462665 ) ) ;
#2726 = EDGE_CURVE ( 'NONE', #5242, #10626, #4773, .T. ) ;
#2727 = CLOSED_SHELL ( 'NONE', ( #6033, #12737, #9025, #2021, #13496, #6623, #3604, #8684, #14834, #3442, #10301, #1159, #11380 ) ) ;
#2728 = AXIS2_PLACEMENT_3D ( 'NONE', #6116, #15241, #6030 ) ;
#2729 = ORIENTED_EDGE ( 'NONE', *, *, #2545, .T. ) ;
#2730 = DIRECTION ( 'NONE',  ( -1.000000000000000000, 0.000000000000000000, 0.000000000000000000 ) ) ;
#2731 = CARTESIAN_POINT ( 'NONE',  ( -45.00000000000000711, 171.6227766016838245, -19.49999999999998224 ) ) ;
#2732 = AXIS2_PLACEMENT_3D ( 'NONE', #4392, #15182, #13954 ) ;
#2733 = CYLINDRICAL_SURFACE ( 'NONE', #3415, 5.000000000000004441 ) ;
#2734 =( LENGTH_UNIT ( ) NAMED_UNIT ( * ) SI_UNIT ( .MILLI., .METRE. ) );
#2735 = FACE_BOUND ( 'NONE', #13791, .T. ) ;
#2736 = VERTEX_POINT ( 'NONE', #10244 ) ;
#2737 = DIRECTION ( 'NONE',  ( 0.000000000000000000, 0.000000000000000000, -1.000000000000000000 ) ) ;
#2738 = AXIS2_PLACEMENT_3D ( 'NONE', #8314, #7091, #15047 ) ;
#2739 = LINE ( 'NONE', #6820, #16011 ) ;
#2740 = VECTOR ( 'NONE', #16391, 1000.000000000000000 ) ;
#2741 = ORIENTED_EDGE ( 'NONE', *, *, #5382, .T. ) ;
#2742 =( NAMED_UNIT ( * ) SI_UNIT ( $, .STERADIAN. ) SOLID_ANGLE_UNIT ( ) );
#2743 = AXIS2_PLACEMENT_3D ( 'NONE', #10908, #116, #4366 ) ;
#2744 = CARTESIAN_POINT ( 'NONE',  ( -32.34996859904739352, 119.7408970890944744, -5.378151393595213214 ) ) ;
#2745 = CIRCLE ( 'NONE', #12641, 2.500000000000000000 ) ;
#2746 = CARTESIAN_POINT ( 'NONE',  ( -38.00000000000000000, 20.00000000000000000, 0.000000000000000000 ) ) ;
#2747 = CARTESIAN_POINT ( 'NONE',  ( -208.0000000000000853, 174.7326106162513497, 0.000000000000000000 ) ) ;
#2748 = CARTESIAN_POINT ( 'NONE',  ( 31.20890926080315353, 18.00000000000000000, -16.64259892333393154 ) ) ;
#2749 = EDGE_CURVE ( 'NONE', #8947, #11114, #1845, .T. ) ;
#2750 = CARTESIAN_POINT ( 'NONE',  ( 22.66736643345232949, 29.84725565559530480, -7.069278529401977984 ) ) ;
#2751 = CARTESIAN_POINT ( 'NONE',  ( -206.3689767832464668, 173.6103877383153531, -4.531616471133038004 ) ) ;
#2752 = DIRECTION ( 'NONE',  ( 0.000000000000000000, 0.000000000000000000, 1.000000000000000000 ) ) ;
#2753 = LINE ( 'NONE', #7973, #6503 ) ;
#2754 = CARTESIAN_POINT ( 'NONE',  ( 24.03488658890935525, 145.8838445361197387, -23.72313757307398419 ) ) ;
#2755 = ORIENTED_EDGE ( 'NONE', *, *, #14042, .T. ) ;
#2756 = CARTESIAN_POINT ( 'NONE',  ( 196.0000000000000000, 167.6227766016838814, -16.92820660268601429 ) ) ;
#2757 = VECTOR ( 'NONE', #5489, 1000.000000000000000 ) ;
#2758 = ORIENTED_EDGE ( 'NONE', *, *, #12197, .T. ) ;
#2759 = DIRECTION ( 'NONE',  ( 0.000000000000000000, 0.000000000000000000, 1.000000000000000000 ) ) ;
#2760 = AXIS2_PLACEMENT_3D ( 'NONE', #15474, #12819, #3354 ) ;
#2761 = DIRECTION ( 'NONE',  ( -0.000000000000000000, -0.000000000000000000, 1.000000000000000000 ) ) ;
#2762 = EDGE_CURVE ( 'NONE', #11801, #11737, #11321, .T. ) ;
#2763 = EDGE_LOOP ( 'NONE', ( #17460, #14468, #9016, #6481 ) ) ;
#2764 = CARTESIAN_POINT ( 'NONE',  ( -14.90344812367316685, 20.00000000000343547, 8.058388986520416353 ) ) ;
#2765 = LINE ( 'NONE', #5591, #10463 ) ;
#2766 = ORIENTED_EDGE ( 'NONE', *, *, #16955, .F. ) ;
#2767 = FACE_OUTER_BOUND ( 'NONE', #10728, .T. ) ;
#2768 = ORIENTED_EDGE ( 'NONE', *, *, #7492, .T. ) ;
#2769 = DIRECTION ( 'NONE',  ( -1.000000000000000000, 0.000000000000000000, 0.000000000000000000 ) ) ;
#2770 = VECTOR ( 'NONE', #3759, 1000.000000000000000 ) ;
#2771 = DIRECTION ( 'NONE',  ( 0.000000000000000000, 1.000000000000000000, 0.000000000000000000 ) ) ;
#2772 = DIRECTION ( 'NONE',  ( 0.9961946980917464334, 0.08715574274764831264, 0.000000000000000000 ) ) ;
#2773 = FACE_OUTER_BOUND ( 'NONE', #6459, .T. ) ;
#2774 = ORIENTED_EDGE ( 'NONE', *, *, #6823, .T. ) ;
#2775 = CARTESIAN_POINT ( 'NONE',  ( 25.30103246056163968, 148.3373224442694891, 23.38426449892925163 ) ) ;
#2776 = ORIENTED_EDGE ( 'NONE', *, *, #9372, .F. ) ;
#2777 = DIRECTION ( 'NONE',  ( 0.000000000000000000, 0.000000000000000000, 1.000000000000000000 ) ) ;
#2778 = DIRECTION ( 'NONE',  ( 1.000000000000000000, 0.000000000000000000, 0.000000000000000000 ) ) ;
#2779 = EDGE_CURVE ( 'NONE', #14060, #5354, #14319, .T. ) ;
#2780 = CARTESIAN_POINT ( 'NONE',  ( 48.00000000000000711, 167.6227766016838530, 5.571800142134975431 ) ) ;
#2781 = EDGE_CURVE ( 'NONE', #7251, #3946, #15477, .T. ) ;
#2782 = AXIS2_PLACEMENT_3D ( 'NONE', #8873, #5076, #17031 ) ;
#2783 = ORIENTED_EDGE ( 'NONE', *, *, #14471, .F. ) ;
#2784 = EDGE_CURVE ( 'NONE', #15700, #10662, #3443, .T. ) ;
#2785 = ORIENTED_EDGE ( 'NONE', *, *, #1979, .T. ) ;
#2786 = CIRCLE ( 'NONE', #3355, 10.00000000000000000 ) ;
#2787 = STYLED_ITEM ( 'NONE', ( #5571 ), #5730 ) ;
#2788 = CARTESIAN_POINT ( 'NONE',  ( 8.956670050029527985, 133.3372912347335841, 14.64653510947197645 ) ) ;
#2789 = VERTEX_POINT ( 'NONE', #2100 ) ;
#2790 = SHAPE_DEFINITION_REPRESENTATION ( #14917, #17442 ) ;
#2791 = CARTESIAN_POINT ( 'NONE',  ( 49.99999999999998579, 191.6227766016837677, -8.071800142134975431 ) ) ;
#2792 = FACE_OUTER_BOUND ( 'NONE', #17024, .T. ) ;
#2793 = PLANE ( 'NONE',  #16096 ) ;
#2794 = CARTESIAN_POINT ( 'NONE',  ( -73.00000000000001421, 171.6227766016838245, 0.000000000000000000 ) ) ;
#2795 = FACE_BOUND ( 'NONE', #4897, .T. ) ;
#2796 = AXIS2_PLACEMENT_3D ( 'NONE', #9390, #2666, #8056 ) ;
#2797 = VERTEX_POINT ( 'NONE', #7500 ) ;
#2798 = CARTESIAN_POINT ( 'NONE',  ( -77.99750410702147008, 202.2831825963720007, -16.88100368216885983 ) ) ;
#2799 = DIRECTION ( 'NONE',  ( 0.000000000000000000, 0.000000000000000000, -1.000000000000000000 ) ) ;
#2800 = CARTESIAN_POINT ( 'NONE',  ( 31.20890926080315353, 19.99999999999999289, -16.64259892333393154 ) ) ;
#2801 = CARTESIAN_POINT ( 'NONE',  ( -3.000000000000000888, 171.6227766016838245, 0.000000000000000000 ) ) ;
#2802 = DIRECTION ( 'NONE',  ( 0.000000000000000000, 0.000000000000000000, -1.000000000000000000 ) ) ;
#2803 = ORIENTED_EDGE ( 'NONE', *, *, #3444, .F. ) ;
#2804 = EDGE_CURVE ( 'NONE', #15613, #5268, #4856, .T. ) ;
#2805 = DIRECTION ( 'NONE',  ( 0.9961946980917461003, 1.067350013832217088E-17, 0.08715574274765162943 ) ) ;
#2806 = AXIS2_PLACEMENT_3D ( 'NONE', #7466, #12875, #16519 ) ;
#2807 = EDGE_LOOP ( 'NONE', ( #651, #12100 ) ) ;
#2808 = AXIS2_PLACEMENT_3D ( 'NONE', #1284, #6690, #15893 ) ;
#2809 = ORIENTED_EDGE ( 'NONE', *, *, #4152, .F. ) ;
#2810 = SHAPE_DEFINITION_REPRESENTATION ( #12375, #6585 ) ;
#2811 = DIRECTION ( 'NONE',  ( 0.000000000000000000, 0.000000000000000000, 1.000000000000000000 ) ) ;
#2812 = DIRECTION ( 'NONE',  ( -1.000000000000000000, -0.000000000000000000, 0.000000000000000000 ) ) ;
#2813 = CARTESIAN_POINT ( 'NONE',  ( -207.2426727481553996, 166.5388791023002852, 0.8050770646283873511 ) ) ;
#2814 = ORIENTED_EDGE ( 'NONE', *, *, #9455, .T. ) ;
#2815 = PLANE ( 'NONE',  #504 ) ;
#2816 = AXIS2_PLACEMENT_3D ( 'NONE', #9799, #14938, #5735 ) ;
#2817 = CARTESIAN_POINT ( 'NONE',  ( -38.00000000000000000, 18.00000000000000355, 0.000000000000000000 ) ) ;
#2818 = AXIS2_PLACEMENT_3D ( 'NONE', #4014, #14796, #10630 ) ;
#2819 = CARTESIAN_POINT ( 'NONE',  ( -27.99999999999998224, 10.00000000000000000, 35.00200000000000244 ) ) ;
#2820 = EDGE_CURVE ( 'NONE', #14506, #4234, #15645, .T. ) ;
#2821 = AXIS2_PLACEMENT_3D ( 'NONE', #8907, #17143, #9086 ) ;
#2822 = CYLINDRICAL_SURFACE ( 'NONE', #15992, 747.9999999999998863 ) ;
#2823 = CARTESIAN_POINT ( 'NONE',  ( 2.749999999999999112, 2.500000000000002220, 0.000000000000000000 ) ) ;
#2824 = ORIENTED_EDGE ( 'NONE', *, *, #12535, .F. ) ;
#2825 = CARTESIAN_POINT ( 'NONE',  ( -50.00000000000000000, 171.6227766016838245, 0.000000000000000000 ) ) ;
#2826 = CARTESIAN_POINT ( 'NONE',  ( -90.80384757729339640, 204.6227766016838245, 0.000000000000000000 ) ) ;
#2827 = ORIENTED_EDGE ( 'NONE', *, *, #1859, .T. ) ;
#2828 = CARTESIAN_POINT ( 'NONE',  ( -32.66708739526796279, 119.0000000000141824, -4.722170599054655860 ) ) ;
#2829 = AXIS2_PLACEMENT_3D ( 'NONE', #6553, #17522, #5406 ) ;
#2830 = DIRECTION ( 'NONE',  ( 0.000000000000000000, 0.000000000000000000, 1.000000000000000000 ) ) ;
#2831 = CARTESIAN_POINT ( 'NONE',  ( -3.000000000000000888, 171.6227766016838245, 20.00000000000000355 ) ) ;
#2832 = CARTESIAN_POINT ( 'NONE',  ( 0.000000000000000000, 0.000000000000000000, 0.000000000000000000 ) ) ;
#2833 = DIRECTION ( 'NONE',  ( -1.000000000000000000, 0.000000000000000000, 0.000000000000000000 ) ) ;
#2834 = DIRECTION ( 'NONE',  ( 0.000000000000000000, 0.000000000000000000, -1.000000000000000000 ) ) ;
#2835 = PLANE ( 'NONE',  #7064 ) ;
#2836 = EDGE_CURVE ( 'NONE', #11548, #9285, #15263, .T. ) ;
#2837 = VERTEX_POINT ( 'NONE', #1131 ) ;
#2838 = DIRECTION ( 'NONE',  ( -1.000000000000000000, -0.000000000000000000, 0.000000000000000000 ) ) ;
#2839 = CIRCLE ( 'NONE', #10420, 2.500000000000002220 ) ;
#2840 = EDGE_LOOP ( 'NONE', ( #6962, #7913, #16156, #16780 ) ) ;
#2841 = DIRECTION ( 'NONE',  ( -1.156482317317868274E-16, 1.000000000000000000, 0.000000000000000000 ) ) ;
#2842 = AXIS2_PLACEMENT_3D ( 'NONE', #9417, #13506, #13766 ) ;
#2843 = EDGE_CURVE ( 'NONE', #17386, #17370, #15829, .T. ) ;
#2844 = DIRECTION ( 'NONE',  ( -0.000000000000000000, -0.000000000000000000, 1.000000000000000000 ) ) ;
#2845 = ORIENTED_EDGE ( 'NONE', *, *, #12069, .T. ) ;
#2846 = ADVANCED_FACE ( 'NONE', ( #15997 ), #8199, .T. ) ;
#2847 = CARTESIAN_POINT ( 'NONE',  ( -14.56452549316047040, 19.99999999999883826, 9.027778560947799846 ) ) ;
#2848 = EDGE_CURVE ( 'NONE', #1696, #5755, #4931, .T. ) ;
#2849 = DIRECTION ( 'NONE',  ( -1.000000000000000000, 0.000000000000000000, 0.000000000000000000 ) ) ;
#2850 = ORIENTED_EDGE ( 'NONE', *, *, #9138, .T. ) ;
#2851 = CARTESIAN_POINT ( 'NONE',  ( 32.00760546193473033, 153.8546784850603615, -27.80828541846619473 ) ) ;
#2852 = CIRCLE ( 'NONE', #3131, 8.000000000000000000 ) ;
#2853 = EDGE_LOOP ( 'NONE', ( #12287, #8763, #9631, #8160 ) ) ;
#2854 = LINE ( 'NONE', #13739, #16594 ) ;
#2855 = CYLINDRICAL_SURFACE ( 'NONE', #1270, 6.000000000000005329 ) ;
#2856 = DIRECTION ( 'NONE',  ( 0.000000000000000000, 0.000000000000000000, 1.000000000000000000 ) ) ;
#2857 = VERTEX_POINT ( 'NONE', #2638 ) ;
#2858 = DIRECTION ( 'NONE',  ( -1.000000000000000000, 0.000000000000000000, 0.000000000000000000 ) ) ;
#2859 = ORIENTED_EDGE ( 'NONE', *, *, #17159, .T. ) ;
#2860 = CARTESIAN_POINT ( 'NONE',  ( 30.37952724349399958, 151.6237922324447709, 26.24958334688938422 ) ) ;
#2861 = ORIENTED_EDGE ( 'NONE', *, *, #1727, .F. ) ;
#2862 = DIRECTION ( 'NONE',  ( -1.000000000000000000, 0.000000000000000000, 0.000000000000000000 ) ) ;
#2863 = CARTESIAN_POINT ( 'NONE',  ( 49.99999999999998579, 151.6227766016839098, -8.071800142134973655 ) ) ;
#2864 = AXIS2_PLACEMENT_3D ( 'NONE', #14635, #2856, #10899 ) ;
#2865 = CARTESIAN_POINT ( 'NONE',  ( -32.65876937324898677, 118.8519199021378938, -4.574127464417287570 ) ) ;
#2866 = ORIENTED_EDGE ( 'NONE', *, *, #14733, .T. ) ;
#2867 = ORIENTED_EDGE ( 'NONE', *, *, #2545, .F. ) ;
#2868 = CARTESIAN_POINT ( 'NONE',  ( 1.559999999999998943, 0.8660254037844428154, -1.499999999999997780 ) ) ;
#2869 = DIRECTION ( 'NONE',  ( 1.000000000000000000, 0.000000000000000000, 0.000000000000000000 ) ) ;
#2870 = ORIENTED_EDGE ( 'NONE', *, *, #11598, .T. ) ;
#2871 = APPLICATION_PROTOCOL_DEFINITION ( 'draft international standard', 'automotive_design', 1998, #14329 ) ;
#2872 = DIRECTION ( 'NONE',  ( -0.000000000000000000, -0.000000000000000000, 1.000000000000000000 ) ) ;
#2873 = CARTESIAN_POINT ( 'NONE',  ( -80.00000000000001421, 196.6227766016838245, -35.00200000000000244 ) ) ;
#2874 = CARTESIAN_POINT ( 'NONE',  ( 48.00000000000000711, 175.6227766016838530, -21.92820660268601074 ) ) ;
#2875 = EDGE_CURVE ( 'NONE', #15013, #15924, #15730, .T. ) ;
#2876 = FACE_OUTER_BOUND ( 'NONE', #9302, .T. ) ;
#2877 = EDGE_CURVE ( 'NONE', #15883, #4234, #17145, .T. ) ;
#2878 = DIRECTION ( 'NONE',  ( 0.000000000000000000, -0.8660254037844413721, -0.4999999999999953371 ) ) ;
#2879 = EDGE_CURVE ( 'NONE', #17378, #1367, #16100, .T. ) ;
#2880 = ORIENTED_EDGE ( 'NONE', *, *, #16290, .F. ) ;
#2881 = CARTESIAN_POINT ( 'NONE',  ( -725.0000000000001137, 129.9999999999995453, 4.999999999999999112 ) ) ;
#2882 = CARTESIAN_POINT ( 'NONE',  ( 30.00000000000000355, 196.6227766016838245, -13.00000000000000000 ) ) ;
#2883 = CARTESIAN_POINT ( 'NONE',  ( -33.99999999999997868, 10.00000000000000000, -16.00000000000000000 ) ) ;
#2884 = CARTESIAN_POINT ( 'NONE',  ( -43.00000000000001421, 125.3137084989847665, -13.00000000000000178 ) ) ;
#2885 = CARTESIAN_POINT ( 'NONE',  ( -725.0000000000000000, 134.2062027339443944, -13.00000000000000000 ) ) ;
#2886 = PRODUCT_DEFINITION_CONTEXT ( 'detailed design', #5517, 'design' ) ;
#2887 = EDGE_LOOP ( 'NONE', ( #13403, #3178, #13306, #5990 ) ) ;
#2888 = LINE ( 'NONE', #8279, #12730 ) ;
#2889 = EDGE_LOOP ( 'NONE', ( #13229, #3520, #8309, #11572 ) ) ;
#2890 = DIRECTION ( 'NONE',  ( 1.000000000000000000, -0.000000000000000000, -0.000000000000000000 ) ) ;
#2891 = EDGE_LOOP ( 'NONE', ( #3034, #15944 ) ) ;
#2892 = CARTESIAN_POINT ( 'NONE',  ( -95.00000000000000000, 143.9321776784423150, -5.086680500673126297E-15 ) ) ;
#2893 = CARTESIAN_POINT ( 'NONE',  ( -100.0000000000000000, 201.9542783778900059, -13.00000000000000000 ) ) ;
#2894 = CARTESIAN_POINT ( 'NONE',  ( -207.7508999721942189, 166.3372983242019529, 1.236577052156976331 ) ) ;
#2895 = ADVANCED_FACE ( 'NONE', ( #6536 ), #9267, .T. ) ;
#2896 = EDGE_CURVE ( 'NONE', #9911, #12513, #15559, .T. ) ;
#2897 = EDGE_CURVE ( 'NONE', #5896, #15148, #11320, .T. ) ;
#2898 = ADVANCED_FACE ( 'NONE', ( #9435 ), #3273, .F. ) ;
#2899 = ORIENTED_EDGE ( 'NONE', *, *, #13334, .T. ) ;
#2900 = DIRECTION ( 'NONE',  ( -0.000000000000000000, -0.000000000000000000, -1.000000000000000000 ) ) ;
#2901 = CARTESIAN_POINT ( 'NONE',  ( -45.00000000000000000, 171.6227766016838245, 0.000000000000000000 ) ) ;
#2902 = DIRECTION ( 'NONE',  ( -1.000000000000000000, 0.000000000000000000, 0.000000000000000000 ) ) ;
#2903 = DIRECTION ( 'NONE',  ( -1.000000000000000000, 0.000000000000000000, 0.000000000000000000 ) ) ;
#2904 = PRODUCT_DEFINITION_SHAPE ( 'NONE', 'NONE',  #4806 ) ;
#2905 = CARTESIAN_POINT ( 'NONE',  ( 21.84350049701297536, 139.6359888969276426, -14.21326463380156646 ) ) ;
#2906 = ORIENTED_EDGE ( 'NONE', *, *, #10774, .F. ) ;
#2907 = FACE_BOUND ( 'NONE', #16814, .T. ) ;
#2908 = CARTESIAN_POINT ( 'NONE',  ( 196.0000000000000000, 183.6227766016837961, -8.071800142134975431 ) ) ;
#2909 = ORIENTED_EDGE ( 'NONE', *, *, #10335, .T. ) ;
#2910 =( NAMED_UNIT ( * ) PLANE_ANGLE_UNIT ( ) SI_UNIT ( $, .RADIAN. ) );
#2911 = CARTESIAN_POINT ( 'NONE',  ( -75.97730433202670497, 192.1516832787069688, -28.34894355864045679 ) ) ;
#2912 = EDGE_CURVE ( 'NONE', #16523, #16282, #290, .T. ) ;
#2913 = DIRECTION ( 'NONE',  ( 0.000000000000000000, 0.000000000000000000, 1.000000000000000000 ) ) ;
#2914 = CARTESIAN_POINT ( 'NONE',  ( 30.40149590727984830, 191.6349927435749407, 26.23951396249186274 ) ) ;
#2915 = CARTESIAN_POINT ( 'NONE',  ( -77.50000000000002842, 146.6227766016838245, 1.387778780781445676E-14 ) ) ;
#2916 = CARTESIAN_POINT ( 'NONE',  ( -18.25212770525996930, 32.30769230769230660, -15.00000000000000000 ) ) ;
#2917 = DIRECTION ( 'NONE',  ( -1.156482317317868274E-16, 1.000000000000000000, 0.000000000000000000 ) ) ;
#2918 = CARTESIAN_POINT ( 'NONE',  ( 12.11856678106299512, 143.7750213247282431, -17.70723251555758537 ) ) ;
#2919 = FACE_BOUND ( 'NONE', #8659, .T. ) ;
#2920 = ORIENTED_EDGE ( 'NONE', *, *, #16954, .F. ) ;
#2921 = CARTESIAN_POINT ( 'NONE',  ( -9.825395436088792067, 30.54854208321445341, -14.75250191942001088 ) ) ;
#2922 = VERTEX_POINT ( 'NONE', #5385 ) ;
#2923 = DIRECTION ( 'NONE',  ( 0.000000000000000000, 0.000000000000000000, -1.000000000000000000 ) ) ;
#2924 = DIRECTION ( 'NONE',  ( 1.000000000000000000, 0.000000000000000000, 0.000000000000000000 ) ) ;
#2925 = ORIENTED_EDGE ( 'NONE', *, *, #3825, .F. ) ;
#2926 = CARTESIAN_POINT ( 'NONE',  ( -22.80699178664306004, 19.99999999999999645, 18.33022619056923119 ) ) ;
#2927 = DIRECTION ( 'NONE',  ( -1.000000000000000000, -0.000000000000000000, -0.000000000000000000 ) ) ;
#2928 = ORIENTED_EDGE ( 'NONE', *, *, #2726, .T. ) ;
#2929 = CARTESIAN_POINT ( 'NONE',  ( -27.99999999999998224, 10.00000000000000000, -16.00000000000000000 ) ) ;
#2930 = EDGE_CURVE ( 'NONE', #10705, #8790, #10941, .T. ) ;
#2931 = ORIENTED_EDGE ( 'NONE', *, *, #15097, .T. ) ;
#2932 = DIRECTION ( 'NONE',  ( 0.000000000000000000, 0.000000000000000000, 1.000000000000000000 ) ) ;
#2933 = FACE_OUTER_BOUND ( 'NONE', #7986, .T. ) ;
#2934 = DIRECTION ( 'NONE',  ( 1.000000000000000000, 1.156482317317868274E-16, -0.000000000000000000 ) ) ;
#2935 = VERTEX_POINT ( 'NONE', #10853 ) ;
#2936 = DIRECTION ( 'NONE',  ( -1.000000000000000000, -0.000000000000000000, -0.000000000000000000 ) ) ;
#2937 = EDGE_CURVE ( 'NONE', #7044, #14845, #10755, .T. ) ;
#2938 = EDGE_CURVE ( 'NONE', #10721, #4086, #9697, .T. ) ;
#2939 = DIRECTION ( 'NONE',  ( 1.000000000000000000, 0.000000000000000000, 0.000000000000000000 ) ) ;
#2940 = ORIENTED_EDGE ( 'NONE', *, *, #6959, .T. ) ;
#2941 = FACE_BOUND ( 'NONE', #12143, .T. ) ;
#2942 = ORIENTED_EDGE ( 'NONE', *, *, #16368, .F. ) ;
#2943 = CARTESIAN_POINT ( 'NONE',  ( -80.00000000000002842, 146.6227766016838245, 10.00000000000000178 ) ) ;
#2944 = LINE ( 'NONE', #6856, #4981 ) ;
#2945 = CARTESIAN_POINT ( 'NONE',  ( -80.00000000000002842, 146.6227766016838245, 0.000000000000000000 ) ) ;
#2946 = ORIENTED_EDGE ( 'NONE', *, *, #7071, .T. ) ;
#2947 = ORIENTED_EDGE ( 'NONE', *, *, #16713, .T. ) ;
#2948 = CYLINDRICAL_SURFACE ( 'NONE', #14577, 20.00000000000000355 ) ;
#2949 = CIRCLE ( 'NONE', #4652, 20.00000000000000355 ) ;
#2950 = DIRECTION ( 'NONE',  ( -1.000000000000000000, -0.000000000000000000, -0.000000000000000000 ) ) ;
#2951 = CARTESIAN_POINT ( 'NONE',  ( 10.98422133653362920, 132.2143956889292724, 13.95899527751216240 ) ) ;
#2952 = ORIENTED_EDGE ( 'NONE', *, *, #7429, .F. ) ;
#2953 = APPLICATION_PROTOCOL_DEFINITION ( 'draft international standard', 'automotive_design', 1998, #7096 ) ;
#2954 = CARTESIAN_POINT ( 'NONE',  ( -34.99999999999999289, 120.0000000000000284, 4.999999999999999112 ) ) ;
#2955 = LINE ( 'NONE', #8091, #11169 ) ;
#2956 = CARTESIAN_POINT ( 'NONE',  ( 21.29916379186985154, 29.87370047437059384, -9.875089623381150261 ) ) ;
#2957 = DIRECTION ( 'NONE',  ( 1.000000000000000000, 0.000000000000000000, 0.000000000000000000 ) ) ;
#2958 = DIRECTION ( 'NONE',  ( -0.000000000000000000, -0.000000000000000000, -1.000000000000000000 ) ) ;
#2959 = EDGE_CURVE ( 'NONE', #4527, #13322, #15568, .T. ) ;
#2960 = CIRCLE ( 'NONE', #7194, 2.500000000000000444 ) ;
#2961 = ORIENTED_EDGE ( 'NONE', *, *, #9910, .F. ) ;
#2962 = CARTESIAN_POINT ( 'NONE',  ( 40.00000000000000711, 206.6227766016838245, 0.000000000000000000 ) ) ;
#2964 = DIRECTION ( 'NONE',  ( -1.000000000000000000, 0.000000000000000000, 0.000000000000000000 ) ) ;
#2963 = AXIS2_PLACEMENT_3D ( 'NONE', #975, #7444, #6375 ) ;
#2965 = CARTESIAN_POINT ( 'NONE',  ( -168.0000000000000284, 178.2321571572880146, 0.000000000000000000 ) ) ;
#2966 = CARTESIAN_POINT ( 'NONE',  ( -50.00000000000000000, 171.6227766016838245, -2.296212748401287183E-15 ) ) ;
#2967 = VERTEX_POINT ( 'NONE', #12198 ) ;
#2968 = ORIENTED_EDGE ( 'NONE', *, *, #5699, .F. ) ;
#2969 = DIRECTION ( 'NONE',  ( 0.000000000000000000, 0.000000000000000000, -1.000000000000000000 ) ) ;
#2970 = EDGE_CURVE ( 'NONE', #4551, #3929, #1563, .T. ) ;
#2971 = ORIENTED_EDGE ( 'NONE', *, *, #281, .T. ) ;
#2972 =( NAMED_UNIT ( * ) PLANE_ANGLE_UNIT ( ) SI_UNIT ( $, .RADIAN. ) );
#2973 = VERTEX_POINT ( 'NONE', #15019 ) ;
#2974 =( NAMED_UNIT ( * ) PLANE_ANGLE_UNIT ( ) SI_UNIT ( $, .RADIAN. ) );
#2975 = CARTESIAN_POINT ( 'NONE',  ( -15.00000000000002487, 120.0000000000000284, 4.999999999999999112 ) ) ;
#2976 = AXIS2_PLACEMENT_3D ( 'NONE', #6722, #6814, #12207 ) ;
#2977 = VECTOR ( 'NONE', #12756, 1000.000000000000000 ) ;
#2978 = CARTESIAN_POINT ( 'NONE',  ( -153.0000000000000284, 183.5597664603500903, 0.000000000000000000 ) ) ;
#2979 = CARTESIAN_POINT ( 'NONE',  ( -197.9999999999999716, 171.6227766016838245, 0.000000000000000000 ) ) ;
#2980 = CARTESIAN_POINT ( 'NONE',  ( 37.20996884815642147, 144.4916047800714978, -18.80562413441371206 ) ) ;
#2981 = ORIENTED_EDGE ( 'NONE', *, *, #16182, .T. ) ;
#2982 = CARTESIAN_POINT ( 'NONE',  ( -23.00000000000002842, 120.0000000000000284, -4.999999999999999112 ) ) ;
#2983 = CARTESIAN_POINT ( 'NONE',  ( 30.00000000000001066, 146.6227766016838245, 0.000000000000000000 ) ) ;
#2984 = CARTESIAN_POINT ( 'NONE',  ( 1.559999999999998943, -0.8660254037844428154, -1.499999999999997780 ) ) ;
#2985 = FACE_OUTER_BOUND ( 'NONE', #3988, .T. ) ;
#2986 = AXIS2_PLACEMENT_3D ( 'NONE', #2978, #5729, #8206 ) ;
#2987 = CIRCLE ( 'NONE', #15139, 2.500000000000002220 ) ;
#2988 = CARTESIAN_POINT ( 'NONE',  ( 13.66217116581496249, 130.1207327347060527, -12.31521373833130717 ) ) ;
#2989 = EDGE_CURVE ( 'NONE', #1199, #13489, #66, .T. ) ;
#2990 = EDGE_CURVE ( 'NONE', #11907, #13275, #11597, .T. ) ;
#2991 = EDGE_CURVE ( 'NONE', #15814, #10603, #9332, .T. ) ;
#2992 = ORIENTED_EDGE ( 'NONE', *, *, #5206, .F. ) ;
#2993 = FACE_BOUND ( 'NONE', #10684, .T. ) ;
#2994 = DIRECTION ( 'NONE',  ( -0.08715574274764689711, 0.9961946980917465444, 0.000000000000000000 ) ) ;
#2995 = ORIENTED_EDGE ( 'NONE', *, *, #1705, .T. ) ;
#2996 =( LENGTH_UNIT ( ) NAMED_UNIT ( * ) SI_UNIT ( .MILLI., .METRE. ) );
#2997 = DIRECTION ( 'NONE',  ( -1.000000000000000000, -6.938893903907228378E-16, -0.000000000000000000 ) ) ;
#2998 = AXIS2_PLACEMENT_3D ( 'NONE', #8861, #13038, #11524 ) ;
#2999 = DIRECTION ( 'NONE',  ( -1.000000000000000000, -0.000000000000000000, -0.000000000000000000 ) ) ;
#3000 = CIRCLE ( 'NONE', #1012, 7.499999999999996447 ) ;
#3001 = DIRECTION ( 'NONE',  ( 0.000000000000000000, -1.000000000000000000, 0.000000000000000000 ) ) ;
#3002 = LINE ( 'NONE', #8400, #961 ) ;
#3003 = CARTESIAN_POINT ( 'NONE',  ( 48.00000000000000711, 175.6227766016838530, 16.92820660268601429 ) ) ;
#3004 = CARTESIAN_POINT ( 'NONE',  ( -95.00000000000000000, 199.3133755249253056, 1.695560166891042033E-15 ) ) ;
#3005 = DIRECTION ( 'NONE',  ( 0.000000000000000000, 0.000000000000000000, 1.000000000000000000 ) ) ;
#3006 = B_SPLINE_CURVE_WITH_KNOTS ( 'NONE', 3,
 ( #12809, #16719, #12463, #13967, #1829, #1920, #2980, #9965, #679, #8377 ),
 .UNSPECIFIED., .F., .F.,
 ( 4, 2, 2, 2, 4 ),
 ( 2.030441771438897272E-17, 0.002588446031580681969, 0.005176892063161337917, 0.007765338094741995600, 0.01035378412632265502 ),
 .UNSPECIFIED. ) ;
#3007 = ORIENTED_EDGE ( 'NONE', *, *, #10791, .T. ) ;
#3008 = ORIENTED_EDGE ( 'NONE', *, *, #7683, .F. ) ;
#3009 = DIRECTION ( 'NONE',  ( -0.000000000000000000, -0.000000000000000000, -1.000000000000000000 ) ) ;
#3010 = CIRCLE ( 'NONE', #10354, 2.499999999999998668 ) ;
#3011 = CARTESIAN_POINT ( 'NONE',  ( -86.00000000000001421, 196.6227766016838245, -35.00000000000000000 ) ) ;
#3012 = AXIS2_PLACEMENT_3D ( 'NONE', #7082, #10872, #13816 ) ;
#3013 = EDGE_LOOP ( 'NONE', ( #12312, #16569, #9690, #2870 ) ) ;
#3014 = DIRECTION ( 'NONE',  ( 0.000000000000000000, 0.000000000000000000, -1.000000000000000000 ) ) ;
#3015 = AXIS2_PLACEMENT_3D ( 'NONE', #17080, #10522, #5040 ) ;
#3016 = CARTESIAN_POINT ( 'NONE',  ( -80.00000000000002842, 146.6227766016838245, 0.000000000000000000 ) ) ;
#3017 = VERTEX_POINT ( 'NONE', #8374 ) ;
#3018 = CARTESIAN_POINT ( 'NONE',  ( 22.50000000000001421, 146.6227766016838245, -21.54065922853802562 ) ) ;
#3019 = DIRECTION ( 'NONE',  ( 0.000000000000000000, 0.000000000000000000, 1.000000000000000000 ) ) ;
#3020 = DIRECTION ( 'NONE',  ( -1.000000000000000000, -0.000000000000000000, 0.000000000000000000 ) ) ;
#3021 = CARTESIAN_POINT ( 'NONE',  ( -100.0000000000000000, 171.6227766016838245, 0.000000000000000000 ) ) ;
#3022 = CARTESIAN_POINT ( 'NONE',  ( -24.94987437106621542, 20.00000000000004263, 5.999999999999992895 ) ) ;
#3023 = CIRCLE ( 'NONE', #12926, 6.000000000000005329 ) ;
#3024 = DIRECTION ( 'NONE',  ( 0.000000000000000000, 0.000000000000000000, -1.000000000000000000 ) ) ;
#3025 =( GEOMETRIC_REPRESENTATION_CONTEXT ( 3 ) GLOBAL_UNCERTAINTY_ASSIGNED_CONTEXT ( ( #7361 ) ) GLOBAL_UNIT_ASSIGNED_CONTEXT ( ( #7140, #5383, #2721 ) ) REPRESENTATION_CONTEXT ( 'NONE', 'WORKASPACE' ) );
#3026 = DIRECTION ( 'NONE',  ( 1.000000000000000000, 0.000000000000000000, -0.000000000000000000 ) ) ;
#3027 = ORIENTED_EDGE ( 'NONE', *, *, #11645, .T. ) ;
#3028 =( REPRESENTATION_RELATIONSHIP ('NONE','NONE', #9723, #6585 ) REPRESENTATION_RELATIONSHIP_WITH_TRANSFORMATION ( #11270 )SHAPE_REPRESENTATION_RELATIONSHIP( ) );
#3029 = VERTEX_POINT ( 'NONE', #328 ) ;
#3030 = EDGE_CURVE ( 'NONE', #10869, #102, #13593, .T. ) ;
#3031 = DIRECTION ( 'NONE',  ( -0.000000000000000000, -0.000000000000000000, 1.000000000000000000 ) ) ;
#3032 = DIRECTION ( 'NONE',  ( 0.000000000000000000, 1.000000000000000000, 0.000000000000000000 ) ) ;
#3033 = CYLINDRICAL_SURFACE ( 'NONE', #7235, 33.00000000000000000 ) ;
#3034 = ORIENTED_EDGE ( 'NONE', *, *, #7584, .F. ) ;
#3035 = EDGE_LOOP ( 'NONE', ( #12238, #2184 ) ) ;
#3036 = CARTESIAN_POINT ( 'NONE',  ( 30.49999999999998224, 9.999999999999998224, -16.00000000000000000 ) ) ;
#3037 = AXIS2_PLACEMENT_3D ( 'NONE', #12372, #71, #5649 ) ;
#3038 = CARTESIAN_POINT ( 'NONE',  ( 196.0000000000000000, 167.6227766016838814, -19.42820660268601074 ) ) ;
#3039 = CARTESIAN_POINT ( 'NONE',  ( 27.44407568426053246, 138.8271129316868837, -3.666666666666671404 ) ) ;
#3040 = CARTESIAN_POINT ( 'NONE',  ( 17.54349574104657705, 125.4948194589026684, 5.000000000000002665 ) ) ;
#3041 = ORIENTED_EDGE ( 'NONE', *, *, #9973, .F. ) ;
#3042 = DIRECTION ( 'NONE',  ( 0.000000000000000000, 0.000000000000000000, -1.000000000000000000 ) ) ;
#3043 = DIRECTION ( 'NONE',  ( -1.000000000000000000, 0.000000000000000000, 0.000000000000000000 ) ) ;
#3044 = CARTESIAN_POINT ( 'NONE',  ( 22.66773460012013430, 29.84724857135450193, -7.067878044979525320 ) ) ;
#3045 = CARTESIAN_POINT ( 'NONE',  ( -194.2319660531761656, 171.6227766016838245, 19.01029467089431080 ) ) ;
#3046 = CARTESIAN_POINT ( 'NONE',  ( 16.23725950538872809, 18.00000000000000000, 24.99999999982344789 ) ) ;
#3047 = CARTESIAN_POINT ( 'NONE',  ( -27.70723240392776532, 19.99999999999999289, 8.328409877367407788 ) ) ;
#3048 = ORIENTED_EDGE ( 'NONE', *, *, #8512, .F. ) ;
#3049 = CARTESIAN_POINT ( 'NONE',  ( 30.00000000000000355, 196.6227766016838245, 11.50215154306610188 ) ) ;
#3050 = VECTOR ( 'NONE', #663, 1000.000000000000000 ) ;
#3051 = CARTESIAN_POINT ( 'NONE',  ( 48.00000000000000711, 179.6227766016838245, 15.00000337241049486 ) ) ;
#3052 = CARTESIAN_POINT ( 'NONE',  ( 39.99999999999999289, 8.000000000000000000, -35.00000000000002132 ) ) ;
#3053 = ADVANCED_FACE ( 'NONE', ( #5728 ), #11117, .T. ) ;
#3054 = DIRECTION ( 'NONE',  ( -0.000000000000000000, -0.000000000000000000, -1.000000000000000000 ) ) ;
#3055 = AXIS2_PLACEMENT_3D ( 'NONE', #7290, #653, #3634 ) ;
#3056 = CARTESIAN_POINT ( 'NONE',  ( -70.00000000000000000, 206.6227766016838245, 2.143131898507868248E-15 ) ) ;
#3057 = ORIENTED_EDGE ( 'NONE', *, *, #10246, .F. ) ;
#3058 = ORIENTED_EDGE ( 'NONE', *, *, #12376, .T. ) ;
#3059 = EDGE_CURVE ( 'NONE', #15769, #11112, #12464, .T. ) ;
#3060 = CARTESIAN_POINT ( 'NONE',  ( -27.98221281347037959, 30.00000000000000000, -15.00000000000000000 ) ) ;
#3061 = VERTEX_POINT ( 'NONE', #14840 ) ;
#3062 = EDGE_CURVE ( 'NONE', #8265, #8813, #2722, .T. ) ;
#3063 = FILL_AREA_STYLE ('',( #3238 ) ) ;
#3064 = EDGE_CURVE ( 'NONE', #14627, #9221, #18, .T. ) ;
#3065 = VERTEX_POINT ( 'NONE', #12724 ) ;
#3066 =( NAMED_UNIT ( * ) SI_UNIT ( $, .STERADIAN. ) SOLID_ANGLE_UNIT ( ) );
#3067 = CIRCLE ( 'NONE', #15787, 2.500000000000000000 ) ;
#3068 = CARTESIAN_POINT ( 'NONE',  ( 0.000000000000000000, 0.000000000000000000, 0.000000000000000000 ) ) ;
#3069 = CIRCLE ( 'NONE', #15222, 2.500000000000000000 ) ;
#3070 = DIRECTION ( 'NONE',  ( 1.000000000000000000, -0.000000000000000000, -0.000000000000000000 ) ) ;
#3071 = DIRECTION ( 'NONE',  ( -1.000000000000000000, 0.000000000000000000, 0.000000000000000000 ) ) ;
#3072 = B_SPLINE_CURVE_WITH_KNOTS ( 'NONE', 3,
 ( #13837, #1701, #7098, #363, #16572, #8509, #12934, #14343, #9996, #8688 ),
 .UNSPECIFIED., .F., .F.,
 ( 4, 2, 2, 2, 4 ),
 ( 0.03775390620236029199, 0.04033669301524710205, 0.04291947982813391210, 0.04550226664102072216, 0.04808505345390753222 ),
 .UNSPECIFIED. ) ;
#3073 = FACE_OUTER_BOUND ( 'NONE', #8687, .T. ) ;
#3074 = CARTESIAN_POINT ( 'NONE',  ( 32.90650748920769075, 18.00000000000000000, -13.87185692903161360 ) ) ;
#3075 = ORIENTED_EDGE ( 'NONE', *, *, #16199, .F. ) ;
#3076 = CARTESIAN_POINT ( 'NONE',  ( 34.78753451919190098, 145.1525832006840631, 19.71138291685209154 ) ) ;
#3077 = FACE_OUTER_BOUND ( 'NONE', #3670, .T. ) ;
#3078 = EDGE_CURVE ( 'NONE', #6948, #14253, #5806, .T. ) ;
#3079 = FACE_BOUND ( 'NONE', #524, .T. ) ;
#3080 = DIRECTION ( 'NONE',  ( 1.000000000000000000, 0.000000000000000000, -0.000000000000000000 ) ) ;
#3081 = AXIS2_PLACEMENT_3D ( 'NONE', #13874, #14044, #3327 ) ;
#3082 = CIRCLE ( 'NONE', #13271, 24.99999999999999645 ) ;
#3083 = DIRECTION ( 'NONE',  ( -1.000000000000000000, 0.000000000000000000, 0.000000000000000000 ) ) ;
#3084 = ORIENTED_EDGE ( 'NONE', *, *, #15675, .F. ) ;
#3085 = FACE_OUTER_BOUND ( 'NONE', #11269, .T. ) ;
#3086 = EDGE_LOOP ( 'NONE', ( #13012, #5925 ) ) ;
#3087 = FILL_AREA_STYLE_COLOUR ( '', #9802 ) ;
#3088 = DIRECTION ( 'NONE',  ( 1.000000000000000000, 0.000000000000000000, 0.000000000000000000 ) ) ;
#3089 = DIRECTION ( 'NONE',  ( 0.000000000000000000, 0.000000000000000000, 1.000000000000000000 ) ) ;
#3090 = AXIS2_PLACEMENT_3D ( 'NONE', #16541, #15024, #16633 ) ;
#3091 = VECTOR ( 'NONE', #3472, 1000.000000000000000 ) ;
#3092 = CARTESIAN_POINT ( 'NONE',  ( 30.79456682210174634, 191.6823464236538541, 26.20333082749370135 ) ) ;
#3093 = AXIS2_PLACEMENT_3D ( 'NONE', #10503, #11735, #5525 ) ;
#3094 = DIRECTION ( 'NONE',  ( 0.000000000000000000, 0.000000000000000000, -1.000000000000000000 ) ) ;
#3095 = DIRECTION ( 'NONE',  ( 0.9961946980917465444, -0.04357787137382451714, 0.07547908730516460218 ) ) ;
#3096 = LINE ( 'NONE', #16557, #7039 ) ;
#3097 = ADVANCED_FACE ( 'NONE', ( #16878 ), #7403, .F. ) ;
#3098 = EDGE_CURVE ( 'NONE', #4046, #9326, #5995, .T. ) ;
#3099 = LINE ( 'NONE', #15392, #1981 ) ;
#3100 = EDGE_CURVE ( 'NONE', #2211, #5446, #15287, .T. ) ;
#3101 = FACE_BOUND ( 'NONE', #11966, .T. ) ;
#3102 = ORIENTED_EDGE ( 'NONE', *, *, #2022, .F. ) ;
#3103 = ORIENTED_EDGE ( 'NONE', *, *, #7492, .F. ) ;
#3104 = CARTESIAN_POINT ( 'NONE',  ( 34.80444759362561058, 19.99999999999999645, -7.621511755370173447 ) ) ;
#3105 = CYLINDRICAL_SURFACE ( 'NONE', #5843, 12.00000000000000000 ) ;
#3106 = ORIENTED_EDGE ( 'NONE', *, *, #4473, .F. ) ;
#3107 = CARTESIAN_POINT ( 'NONE',  ( -13.51825462539708056, 19.99999999999884892, 10.94502331224290259 ) ) ;
#3108 = VECTOR ( 'NONE', #2997, 1000.000000000000000 ) ;
#3109 = CYLINDRICAL_SURFACE ( 'NONE', #12742, 2.500000000000000444 ) ;
#3110 = ORIENTED_EDGE ( 'NONE', *, *, #4202, .F. ) ;
#3111 = CARTESIAN_POINT ( 'NONE',  ( -153.0000000000000284, 171.6227766016838245, -21.61734737250326077 ) ) ;
#3112 = DIRECTION ( 'NONE',  ( 0.000000000000000000, 0.000000000000000000, -1.000000000000000000 ) ) ;
#3113 = FACE_OUTER_BOUND ( 'NONE', #12070, .T. ) ;
#3114 = FACE_OUTER_BOUND ( 'NONE', #11893, .T. ) ;
#3115 = VECTOR ( 'NONE', #1352, 1000.000000000000000 ) ;
#3116 = AXIS2_PLACEMENT_3D ( 'NONE', #8384, #7067, #7149 ) ;
#3117 = FACE_OUTER_BOUND ( 'NONE', #9378, .T. ) ;
#3118 = EDGE_CURVE ( 'NONE', #14929, #4566, #3339, .T. ) ;
#3119 = CARTESIAN_POINT ( 'NONE',  ( 24.72505082391213804, 141.2912748254776147, -13.00000000000000000 ) ) ;
#3120 = AXIS2_PLACEMENT_3D ( 'NONE', #16364, #4317, #4403 ) ;
#3121 = EDGE_CURVE ( 'NONE', #453, #7418, #7700, .T. ) ;
#3122 = DIRECTION ( 'NONE',  ( -1.156482317317868274E-16, 1.000000000000000000, 0.000000000000000000 ) ) ;
#3123 = ORIENTED_EDGE ( 'NONE', *, *, #4202, .T. ) ;
#3124 = FACE_BOUND ( 'NONE', #13387, .T. ) ;
#3125 = EDGE_LOOP ( 'NONE', ( #5478, #12634, #10559, #14036 ) ) ;
#3126 = DIRECTION ( 'NONE',  ( -0.000000000000000000, -1.000000000000000000, 2.312964634635742267E-15 ) ) ;
#3127 = CARTESIAN_POINT ( 'NONE',  ( -7.379000772445021283, 30.00000000000000000, -13.00000000000000000 ) ) ;
#3128 = EDGE_LOOP ( 'NONE', ( #16767, #4880, #6389 ) ) ;
#3129 = VERTEX_POINT ( 'NONE', #2008 ) ;
#3130 = CARTESIAN_POINT ( 'NONE',  ( -80.00000000000001421, 196.6227766016838245, 35.00200000000000244 ) ) ;
#3131 = AXIS2_PLACEMENT_3D ( 'NONE', #6029, #10323, #8270 ) ;
#3132 = LINE ( 'NONE', #16591, #4516 ) ;
#3133 = CARTESIAN_POINT ( 'NONE',  ( 16.78995144247101123, 126.8031893778130410, 8.318227863269529010 ) ) ;
#3134 = VECTOR ( 'NONE', #1541, 1000.000000000000000 ) ;
#3135 = ORIENTED_EDGE ( 'NONE', *, *, #11106, .F. ) ;
#3136 = CONTEXT_DEPENDENT_SHAPE_REPRESENTATION ( #11164, #12668 ) ;
#3137 = CARTESIAN_POINT ( 'NONE',  ( 39.99999999999998579, 8.000000000000007105, 30.00000000000001066 ) ) ;
#3138 = ADVANCED_FACE ( 'NONE', ( #12806 ), #11299, .T. ) ;
#3139 = CARTESIAN_POINT ( 'NONE',  ( -3.000000000000000888, 154.3022685259950038, -9.999999999999900524 ) ) ;
#3140 = CARTESIAN_POINT ( 'NONE',  ( -85.00000000000001421, 196.1091490972146119, 22.13677318565945740 ) ) ;
#3141 = DIRECTION ( 'NONE',  ( 0.000000000000000000, 2.891205793294675861E-16, 1.000000000000000000 ) ) ;
#3142 = APPLICATION_CONTEXT ( 'automotive_design' ) ;
#3143 = CARTESIAN_POINT ( 'NONE',  ( 16.75727253400481942, 18.00000000000057199, 12.82782196133976704 ) ) ;
#3144 = PLANE ( 'NONE',  #14534 ) ;
#3145 = ORIENTED_EDGE ( 'NONE', *, *, #4525, .F. ) ;
#3146 = LINE ( 'NONE', #8623, #12378 ) ;
#3147 = VECTOR ( 'NONE', #14915, 1000.000000000000000 ) ;
#3148 = CARTESIAN_POINT ( 'NONE',  ( -3.000000000000000888, 171.6227766016838245, -20.00000000000000355 ) ) ;
#3149 = LINE ( 'NONE', #228, #15108 ) ;
#3150 = CARTESIAN_POINT ( 'NONE',  ( 32.50000000000000000, 196.6227766016838245, 1.387778780781445676E-14 ) ) ;
#3151 = CARTESIAN_POINT ( 'NONE',  ( 15.00000000000000000, 154.3022685259950038, -9.999999999999900524 ) ) ;
#3152 = ORIENTED_EDGE ( 'NONE', *, *, #11462, .F. ) ;
#3153 = ORIENTED_EDGE ( 'NONE', *, *, #13035, .F. ) ;
#3154 = ORIENTED_EDGE ( 'NONE', *, *, #11923, .F. ) ;
#3155 = CARTESIAN_POINT ( 'NONE',  ( 15.42236477930291549, 143.2198172345435410, 16.80652640733168823 ) ) ;
#3156 = ORIENTED_EDGE ( 'NONE', *, *, #3757, .F. ) ;
#3157 =( LENGTH_UNIT ( ) NAMED_UNIT ( * ) SI_UNIT ( .MILLI., .METRE. ) );
#3158 = CIRCLE ( 'NONE', #9935, 19.49999999999998934 ) ;
#3159 = ORIENTED_EDGE ( 'NONE', *, *, #12950, .T. ) ;
#3160 =( LENGTH_UNIT ( ) NAMED_UNIT ( * ) SI_UNIT ( .MILLI., .METRE. ) );
#3161 = CARTESIAN_POINT ( 'NONE',  ( 30.00000000000000355, 196.6227766016838245, -35.00200000000000244 ) ) ;
#3162 = EDGE_CURVE ( 'NONE', #254, #2477, #11202, .T. ) ;
#3163 =( LENGTH_UNIT ( ) NAMED_UNIT ( * ) SI_UNIT ( .MILLI., .METRE. ) );
#3164 = DIRECTION ( 'NONE',  ( 1.000000000000000000, 0.000000000000000000, 0.000000000000000000 ) ) ;
#3165 = DIRECTION ( 'NONE',  ( 0.000000000000000000, -0.8660254037844413721, -0.4999999999999953371 ) ) ;
#3166 = ORIENTED_EDGE ( 'NONE', *, *, #8022, .T. ) ;
#3167 = CARTESIAN_POINT ( 'NONE',  ( 32.06308580867288072, 142.0644190903623496, 14.67410160148081211 ) ) ;
#3168 = ADVANCED_FACE ( 'NONE', ( #6070 ), #11465, .F. ) ;
#3169 = DIRECTION ( 'NONE',  ( -1.000000000000000000, -0.000000000000000000, -0.000000000000000000 ) ) ;
#3170 = FACE_BOUND ( 'NONE', #10254, .T. ) ;
#3171 = EDGE_CURVE ( 'NONE', #2857, #14947, #15625, .T. ) ;
#3172 = DIRECTION ( 'NONE',  ( 0.000000000000000000, 0.000000000000000000, -1.000000000000000000 ) ) ;
#3173 = EDGE_CURVE ( 'NONE', #1460, #13560, #8889, .T. ) ;
#3174 =( BOUNDED_SURFACE ( )  B_SPLINE_SURFACE ( 3, 2, ( 
 ( #7922, #15708, #930 ),
 ( #13328, #2428, #1192 ),
 ( #6597, #11988, #10663 ),
 ( #8980, #16074, #7827 ) ),
 .UNSPECIFIED., .F., .F., .F. ) 
 B_SPLINE_SURFACE_WITH_KNOTS ( ( 4, 4 ),
 ( 3, 3 ),
 ( 0.1516087691302821228, 0.1566150273425061523 ),
 ( 0.000000000000000000, 1.000000000000000000 ),
 .UNSPECIFIED. ) 
 GEOMETRIC_REPRESENTATION_ITEM ( )  RATIONAL_B_SPLINE_SURFACE ( (
 ( 1.000000000000000000, 0.6556320892438535219, 1.000000000000000000),
 ( 1.000000000000000000, 0.6556321914870770762, 1.000000000000000000),
 ( 1.000000000000000000, 0.6556957163104851771, 1.000000000000000000),
 ( 1.000000000000000000, 0.6558243695371216431, 1.000000000000000000) ) ) 
 REPRESENTATION_ITEM ( '' )  SURFACE ( )  );
#3175 = CARTESIAN_POINT ( 'NONE',  ( -27.99999999999998224, 10.00000000000000000, -16.00000000000000000 ) ) ;
#3176 = ORIENTED_EDGE ( 'NONE', *, *, #4744, .F. ) ;
#3177 = FACE_OUTER_BOUND ( 'NONE', #12170, .T. ) ;
#3178 = ORIENTED_EDGE ( 'NONE', *, *, #4303, .T. ) ;
#3179 =( NAMED_UNIT ( * ) SI_UNIT ( $, .STERADIAN. ) SOLID_ANGLE_UNIT ( ) );
#3180 = DIRECTION ( 'NONE',  ( -0.000000000000000000, -0.000000000000000000, 1.000000000000000000 ) ) ;
#3181 = CARTESIAN_POINT ( 'NONE',  ( 27.48361012698968864, 138.6227766016838245, 1.063447695028166570E-14 ) ) ;
#3182 = CARTESIAN_POINT ( 'NONE',  ( 25.35096429952119834, 194.7608640721562949, 23.53240337055841991 ) ) ;
#3183 = DIRECTION ( 'NONE',  ( -1.000000000000000000, -0.000000000000000000, -0.000000000000000000 ) ) ;
#3184 = CARTESIAN_POINT ( 'NONE',  ( -70.00000000000000000, 171.6227766016838245, 0.000000000000000000 ) ) ;
#3185 = CARTESIAN_POINT ( 'NONE',  ( 18.47699279854304777, 29.92902263789611439, 12.17729482734268132 ) ) ;
#3186 = CARTESIAN_POINT ( 'NONE',  ( 30.00000000000000355, 196.6227766016838245, 0.000000000000000000 ) ) ;
#3187 =( NAMED_UNIT ( * ) SI_UNIT ( $, .STERADIAN. ) SOLID_ANGLE_UNIT ( ) );
#3188 = VERTEX_POINT ( 'NONE', #11557 ) ;
#3189 = EDGE_LOOP ( 'NONE', ( #2167, #14857 ) ) ;
#3190 = CARTESIAN_POINT ( 'NONE',  ( 23.15530394309853435, 20.00000000000112976, -10.88800651875285297 ) ) ;
#3191 = DIRECTION ( 'NONE',  ( -1.000000000000000000, 8.673617379884038430E-16, 0.000000000000000000 ) ) ;
#3192 = ORIENTED_EDGE ( 'NONE', *, *, #13843, .T. ) ;
#3193 = CYLINDRICAL_SURFACE ( 'NONE', #11218, 7.500000000000003553 ) ;
#3194 = DIRECTION ( 'NONE',  ( -0.000000000000000000, -0.000000000000000000, 1.000000000000000000 ) ) ;
#3195 = EDGE_LOOP ( 'NONE', ( #5727, #113, #12363, #1294 ) ) ;
#3196 = EDGE_CURVE ( 'NONE', #9392, #11298, #2574, .T. ) ;
#3197 = PRODUCT ( 'gear selector switch', 'gear selector switch', '', ( #1280 ) ) ;
#3198 = CARTESIAN_POINT ( 'NONE',  ( 24.91549491446250286, 152.1614365523548713, -26.65369102675423818 ) ) ;
#3199 = DIRECTION ( 'NONE',  ( -0.000000000000000000, -0.000000000000000000, -1.000000000000000000 ) ) ;
#3200 = CARTESIAN_POINT ( 'NONE',  ( -68.00000000000000000, 206.6227766016838245, -2.143131898507868248E-15 ) ) ;
#3201 = CARTESIAN_POINT ( 'NONE',  ( -27.98221281347037959, 20.00000000000000000, -15.00000000000000000 ) ) ;
#3202 = DIRECTION ( 'NONE',  ( -1.000000000000000000, -0.000000000000000000, 0.000000000000000000 ) ) ;
#3203 = CARTESIAN_POINT ( 'NONE',  ( -27.99999999999998224, 10.00000000000000000, 1.387778780781445676E-14 ) ) ;
#3204 = DIRECTION ( 'NONE',  ( 0.000000000000000000, 0.000000000000000000, 1.000000000000000000 ) ) ;
#3205 = EDGE_LOOP ( 'NONE', ( #12031, #3572 ) ) ;
#3206 = CARTESIAN_POINT ( 'NONE',  ( -40.00000000000000000, 20.00000000000000000, 30.00000000000000355 ) ) ;
#3207 = EDGE_LOOP ( 'NONE', ( #17376, #7307, #6041, #12589 ) ) ;
#3208 = CARTESIAN_POINT ( 'NONE',  ( 196.0000000000000000, 155.6227766016839098, 12.50000337241049309 ) ) ;
#3209 = FACE_BOUND ( 'NONE', #5928, .T. ) ;
#3210 = VERTEX_POINT ( 'NONE', #16624 ) ;
#3211 = DIRECTION ( 'NONE',  ( 0.000000000000000000, 1.000000000000000000, 0.000000000000000000 ) ) ;
#3212 = ADVANCED_FACE ( 'NONE', ( #4494 ), #9883, .T. ) ;
#3213 = ADVANCED_FACE ( 'NONE', ( #9961, #12977 ), #10389, .F. ) ;
#3214 = DIRECTION ( 'NONE',  ( 0.000000000000000000, 0.000000000000000000, 1.000000000000000000 ) ) ;
#3215 = EDGE_CURVE ( 'NONE', #15544, #5268, #7727, .T. ) ;
#3216 = CARTESIAN_POINT ( 'NONE',  ( 27.25143353317894324, 137.1251711682953385, 6.002437647192902404 ) ) ;
#3217 = VERTEX_POINT ( 'NONE', #7731 ) ;
#3218 = ITEM_DEFINED_TRANSFORMATION ( 'NONE', 'NONE', #12369,  #3583 ) ;
#3219 = FACE_OUTER_BOUND ( 'NONE', #535, .T. ) ;
#3220 = DIRECTION ( 'NONE',  ( -1.000000000000000000, 0.000000000000000000, 0.000000000000000000 ) ) ;
#3221 = DIRECTION ( 'NONE',  ( 1.000000000000000000, 0.000000000000000000, 0.000000000000000000 ) ) ;
#3222 = DIRECTION ( 'NONE',  ( 0.000000000000000000, 0.000000000000000000, 1.000000000000000000 ) ) ;
#3223 = CARTESIAN_POINT ( 'NONE',  ( 17.58250999373989742, 125.2198453306090045, 1.666666666666656749 ) ) ;
#3224 = CARTESIAN_POINT ( 'NONE',  ( -8.720613081040614389, 18.00000000000000000, -24.99999999951824492 ) ) ;
#3225 = VERTEX_POINT ( 'NONE', #7568 ) ;
#3226 = CARTESIAN_POINT ( 'NONE',  ( 30.00000000000001066, 146.6227766016838245, 11.50215154306610188 ) ) ;
#3227 = DIRECTION ( 'NONE',  ( 1.000000000000000000, -0.000000000000000000, -0.000000000000000000 ) ) ;
#3228 = ORIENTED_EDGE ( 'NONE', *, *, #5445, .F. ) ;
#3229 = DIRECTION ( 'NONE',  ( 0.000000000000000000, 0.000000000000000000, 1.000000000000000000 ) ) ;
#3230 = DIRECTION ( 'NONE',  ( -1.000000000000000000, -6.938893903907228378E-16, -0.000000000000000000 ) ) ;
#3231 = CIRCLE ( 'NONE', #13122, 5.000000000000000888 ) ;
#3232 = ORIENTED_EDGE ( 'NONE', *, *, #16711, .F. ) ;
#3233 = CIRCLE ( 'NONE', #409, 23.57392898041431195 ) ;
#3234 = VERTEX_POINT ( 'NONE', #11715 ) ;
#3235 = ORIENTED_EDGE ( 'NONE', *, *, #8316, .F. ) ;
#3236 = CARTESIAN_POINT ( 'NONE',  ( -95.00000000000000000, 143.9321776784423150, -5.086680500673126297E-15 ) ) ;
#3237 = ORIENTED_EDGE ( 'NONE', *, *, #15267, .F. ) ;
#3238 = FILL_AREA_STYLE_COLOUR ( '', #16617 ) ;
#3239 = ORIENTED_EDGE ( 'NONE', *, *, #6135, .F. ) ;
#3240 = CARTESIAN_POINT ( 'NONE',  ( -85.00000000000002842, 196.6227766016838245, 35.00200000000000244 ) ) ;
#3241 = DIRECTION ( 'NONE',  ( 0.000000000000000000, 0.000000000000000000, -1.000000000000000000 ) ) ;
#3242 = AXIS2_PLACEMENT_3D ( 'NONE', #3731, #974, #17089 ) ;
#3243 = CARTESIAN_POINT ( 'NONE',  ( 39.99999999999998579, 0.000000000000000000, -33.00000000000000711 ) ) ;
#3244 = DIRECTION ( 'NONE',  ( 0.000000000000000000, -1.000000000000000000, 6.123233995736762338E-17 ) ) ;
#3245 = CONICAL_SURFACE ( 'NONE', #3812, 2.500000000000002220, 1.029744260000002631 ) ;
#3246 = ORIENTED_EDGE ( 'NONE', *, *, #16042, .T. ) ;
#3247 = CYLINDRICAL_SURFACE ( 'NONE', #14920, 19.49999999999998224 ) ;
#3248 = DIRECTION ( 'NONE',  ( 0.000000000000000000, 8.410780489584519664E-16, 1.000000000000000000 ) ) ;
#3249 = FACE_BOUND ( 'NONE', #5156, .T. ) ;
#3250 = CARTESIAN_POINT ( 'NONE',  ( -11.67692690462290273, 19.99999999999766587, -12.94410612366815272 ) ) ;
#3251 = DIRECTION ( 'NONE',  ( -0.5000000000000042188, 0.000000000000000000, 0.8660254037844361541 ) ) ;
#3252 = ADVANCED_FACE ( 'NONE', ( #15974 ), #11809, .F. ) ;
#3253 = EDGE_CURVE ( 'NONE', #13316, #254, #4910, .T. ) ;
#3254 = CONICAL_SURFACE ( 'NONE', #13144, 2.055000000000000160, 0.7853981633974428389 ) ;
#3255 = CARTESIAN_POINT ( 'NONE',  ( 27.75000000000000000, 0.000000000000000000, 2.055000000000000160 ) ) ;
#3256 = COLOUR_RGB ( '', 0.08235294, 0.09019608, 0.10196078) ;
#3257 = ORIENTED_EDGE ( 'NONE', *, *, #12388, .F. ) ;
#3258 = DIRECTION ( 'NONE',  ( 0.000000000000000000, 1.000000000000000000, 0.000000000000000000 ) ) ;
#3259 = EDGE_LOOP ( 'NONE', ( #14461, #761, #16369, #4885 ) ) ;
#3260 = CARTESIAN_POINT ( 'NONE',  ( 8.602893093599609742, 142.4623620169580818, 19.35743923737696903 ) ) ;
#3261 = ADVANCED_FACE ( 'NONE', ( #2528 ), #3174, .T. ) ;
#3262 = ORIENTED_EDGE ( 'NONE', *, *, #12035, .F. ) ;
#3263 = PLANE ( 'NONE',  #8159 ) ;
#3264 = CARTESIAN_POINT ( 'NONE',  ( 17.00000000000000000, 191.6227766016837961, 1.224646799147353454E-15 ) ) ;
#3265 = AXIS2_PLACEMENT_3D ( 'NONE', #16625, #13965, #3241 ) ;
#3266 = ORIENTED_EDGE ( 'NONE', *, *, #3738, .F. ) ;
#3267 = DIRECTION ( 'NONE',  ( 1.000000000000000000, 0.000000000000000000, 0.000000000000000000 ) ) ;
#3268 = CARTESIAN_POINT ( 'NONE',  ( 48.00000000000000000, 171.6227766016838245, -12.50000337241049131 ) ) ;
#3269 = MECHANICAL_DESIGN_GEOMETRIC_PRESENTATION_REPRESENTATION (  '', ( #157 ), #2416 ) ;
#3270 = DIRECTION ( 'NONE',  ( 1.000000000000000000, 0.000000000000000000, 0.000000000000000000 ) ) ;
#3271 = FILL_AREA_STYLE_COLOUR ( '', #1564 ) ;
#3272 = ORIENTED_EDGE ( 'NONE', *, *, #2836, .F. ) ;
#3273 =( BOUNDED_SURFACE ( )  B_SPLINE_SURFACE ( 3, 2, ( 
 ( #12272, #4138, #13618 ),
 ( #5465, #1486, #8205 ),
 ( #8286, #149, #9525 ),
 ( #5553, #17514, #1661 ) ),
 .UNSPECIFIED., .F., .F., .F. ) 
 B_SPLINE_SURFACE_WITH_KNOTS ( ( 4, 4 ),
 ( 3, 3 ),
 ( 0.1516087691302827056, 0.1566150273425061523 ),
 ( 0.000000000000000000, 1.000000000000000000 ),
 .UNSPECIFIED. ) 
 GEOMETRIC_REPRESENTATION_ITEM ( )  RATIONAL_B_SPLINE_SURFACE ( (
 ( 1.000000000000000000, 0.6556320892438534109, 1.000000000000000000),
 ( 1.000000000000000000, 0.6556321914870764100, 1.000000000000000000),
 ( 1.000000000000000000, 0.6556957163104859543, 1.000000000000000000),
 ( 1.000000000000000000, 0.6558243695371223092, 1.000000000000000000) ) ) 
 REPRESENTATION_ITEM ( '' )  SURFACE ( )  );
#3274 = AXIS2_PLACEMENT_3D ( 'NONE', #5480, #1498, #8297 ) ;
#3275 = VERTEX_POINT ( 'NONE', #3762 ) ;
#3276 = CARTESIAN_POINT ( 'NONE',  ( 30.80964797964808000, 19.99999999999999645, -17.18170494867160514 ) ) ;
#3277 = CARTESIAN_POINT ( 'NONE',  ( -74.72505082391214160, 141.2912748254776147, -13.00000000000000000 ) ) ;
#3278 = ORIENTED_EDGE ( 'NONE', *, *, #3173, .F. ) ;
#3279 = PRODUCT_DEFINITION ( 'UNKNOWN', '', #8129, #4310 ) ;
#3280 = CARTESIAN_POINT ( 'NONE',  ( -73.00000000000001421, 171.6227766016838245, 0.000000000000000000 ) ) ;
#3281 = AXIS2_PLACEMENT_3D ( 'NONE', #1986, #7386, #12784 ) ;
#3282 = EDGE_LOOP ( 'NONE', ( #10040, #8235, #17339, #15031 ) ) ;
#3283 = AXIS2_PLACEMENT_3D ( 'NONE', #14045, #9955, #10291 ) ;
#3284 = PLANE ( 'NONE',  #17232 ) ;
#3285 = EDGE_CURVE ( 'NONE', #4393, #17452, #16707, .T. ) ;
#3286 = ADVANCED_FACE ( 'NONE', ( #15802 ), #1437, .F. ) ;
#3287 = CARTESIAN_POINT ( 'NONE',  ( -27.98221281347037959, 18.00000000000000355, 4.999999999999999112 ) ) ;
#3288 = FACE_OUTER_BOUND ( 'NONE', #16913, .T. ) ;
#3289 = DIRECTION ( 'NONE',  ( 0.000000000000000000, -0.4999999999999952816, -0.8660254037844413721 ) ) ;
#3290 = LINE ( 'NONE', #14101, #1469 ) ;
#3291 = CARTESIAN_POINT ( 'NONE',  ( -32.34996859905196231, 119.7408970890905096, 5.378151393592371043 ) ) ;
#3292 = VECTOR ( 'NONE', #7892, 1000.000000000000000 ) ;
#3293 = DIRECTION ( 'NONE',  ( -1.000000000000000000, -0.000000000000000000, 0.000000000000000000 ) ) ;
#3294 = CIRCLE ( 'NONE', #759, 2.699999999999999289 ) ;
#3295 = ORIENTED_EDGE ( 'NONE', *, *, #6965, .T. ) ;
#3296 = CARTESIAN_POINT ( 'NONE',  ( 27.41872110558518116, 136.9783011792879392, -5.130391642808777242 ) ) ;
#3297 = ADVANCED_FACE ( 'NONE', ( #10486, #9150 ), #14556, .F. ) ;
#3298 = VECTOR ( 'NONE', #15934, 1000.000000000000000 ) ;
#3299 = VERTEX_POINT ( 'NONE', #2791 ) ;
#3300 = CARTESIAN_POINT ( 'NONE',  ( -48.00000000000000000, 154.3022685259950038, -9.999999999999900524 ) ) ;
#3301 = AXIS2_PLACEMENT_3D ( 'NONE', #3612, #10794, #2737 ) ;
#3302 = CARTESIAN_POINT ( 'NONE',  ( -27.98221281347037959, 18.00000000000000355, -4.999999999999999112 ) ) ;
#3303 = ORIENTED_EDGE ( 'NONE', *, *, #6295, .T. ) ;
#3304 = CARTESIAN_POINT ( 'NONE',  ( 29.54149365486396661, 20.00000000000000711, 18.67620474358521676 ) ) ;
#3305 = CARTESIAN_POINT ( 'NONE',  ( 24.02621431236828187, 19.99999999999771916, 9.488192989094725860 ) ) ;
#3306 = CARTESIAN_POINT ( 'NONE',  ( 17.14535223351611748, 126.3036220646326910, 7.355580850454368047 ) ) ;
#3307 = AXIS2_PLACEMENT_3D ( 'NONE', #15748, #14596, #11938 ) ;
#3308 = CIRCLE ( 'NONE', #7822, 5.000000000000006217 ) ;
#3309 = EDGE_LOOP ( 'NONE', ( #23, #15054 ) ) ;
#3310 = ITEM_DEFINED_TRANSFORMATION ( 'NONE', 'NONE', #16616,  #3583 ) ;
#3311 = FACE_OUTER_BOUND ( 'NONE', #740, .T. ) ;
#3312 = VECTOR ( 'NONE', #14242, 1000.000000000000000 ) ;
#3313 =( GEOMETRIC_REPRESENTATION_CONTEXT ( 3 ) GLOBAL_UNCERTAINTY_ASSIGNED_CONTEXT ( ( #6115 ) ) GLOBAL_UNIT_ASSIGNED_CONTEXT ( ( #1398, #13617, #3066 ) ) REPRESENTATION_CONTEXT ( 'NONE', 'WORKASPACE' ) );
#3314 = DIRECTION ( 'NONE',  ( 1.000000000000000000, 0.000000000000000000, 0.000000000000000000 ) ) ;
#3315 = AXIS2_PLACEMENT_3D ( 'NONE', #17142, #12270, #5463 ) ;
#3316 = CARTESIAN_POINT ( 'NONE',  ( -76.71739856777422517, 192.8472041258103218, 25.26942977006890345 ) ) ;
#3317 = DIRECTION ( 'NONE',  ( 1.000000000000000000, 0.000000000000000000, 0.000000000000000000 ) ) ;
#3318 = CYLINDRICAL_SURFACE ( 'NONE', #1326, 2.500000000000000444 ) ;
#3319 = CYLINDRICAL_SURFACE ( 'NONE', #16808, 30.00000000000000000 ) ;
#3320 = ORIENTED_EDGE ( 'NONE', *, *, #4150, .F. ) ;
#3321 = CARTESIAN_POINT ( 'NONE',  ( -75.20964951580667446, 200.2528945340145015, -20.13811431823771159 ) ) ;
#3322 = EDGE_CURVE ( 'NONE', #8608, #3610, #10467, .T. ) ;
#3323 = EDGE_CURVE ( 'NONE', #14499, #7978, #16139, .T. ) ;
#3324 = LINE ( 'NONE', #8721, #16718 ) ;
#3325 = EDGE_CURVE ( 'NONE', #11049, #16267, #1711, .T. ) ;
#3326 = VERTEX_POINT ( 'NONE', #6687 ) ;
#3327 = DIRECTION ( 'NONE',  ( 0.000000000000000000, 1.000000000000000000, 0.000000000000000000 ) ) ;
#3328 = FACE_OUTER_BOUND ( 'NONE', #11942, .T. ) ;
#3329 = ORIENTED_EDGE ( 'NONE', *, *, #991, .F. ) ;
#3330 = EDGE_LOOP ( 'NONE', ( #16952, #4145, #14134, #8499, #1403 ) ) ;
#3331 = ORIENTED_EDGE ( 'NONE', *, *, #3059, .F. ) ;
#3332 = PRODUCT_DEFINITION_FORMATION_WITH_SPECIFIED_SOURCE ( 'ANY', '', #8417, .NOT_KNOWN. ) ;
#3333 = AXIS2_PLACEMENT_3D ( 'NONE', #11530, #6552, #10706 ) ;
#3334 = CARTESIAN_POINT ( 'NONE',  ( 10.03770976535549586, 140.0890479961802839, 11.85997561143382661 ) ) ;
#3335 = ORIENTED_EDGE ( 'NONE', *, *, #6614, .T. ) ;
#3336 = CARTESIAN_POINT ( 'NONE',  ( 48.00000000000000711, 175.6227766016838245, 3.071800142134975431 ) ) ;
#3337 = ORIENTED_EDGE ( 'NONE', *, *, #3864, .T. ) ;
#3338 = FILL_AREA_STYLE ('',( #15545 ) ) ;
#3339 = LINE ( 'NONE', #11385, #590 ) ;
#3340 = DIRECTION ( 'NONE',  ( 0.000000000000000000, 0.000000000000000000, -1.000000000000000000 ) ) ;
#3341 = LINE ( 'NONE', #5814, #722 ) ;
#3342 = AXIS2_PLACEMENT_3D ( 'NONE', #10122, #16781, #390 ) ;
#3343 = AXIS2_PLACEMENT_3D ( 'NONE', #9331, #16164, #16432 ) ;
#3344 = ORIENTED_EDGE ( 'NONE', *, *, #1052, .T. ) ;
#3345 = DIRECTION ( 'NONE',  ( -1.000000000000000000, -0.000000000000000000, -0.000000000000000000 ) ) ;
#3346 = FACE_OUTER_BOUND ( 'NONE', #5110, .T. ) ;
#3347 = EDGE_CURVE ( 'NONE', #9730, #4275, #12746, .T. ) ;
#3348 = CARTESIAN_POINT ( 'NONE',  ( 22.50000000000000000, 196.6227766016838245, -13.00000000000000000 ) ) ;
#3349 = CARTESIAN_POINT ( 'NONE',  ( -7.379000772444995526, 30.00000000000000000, -15.00000000000000355 ) ) ;
#3350 = SURFACE_STYLE_USAGE ( .BOTH. , #11477 ) ;
#3351 = CARTESIAN_POINT ( 'NONE',  ( -3.000000000000000888, 206.6227766016838245, -2.143131898507868248E-15 ) ) ;
#3352 = VECTOR ( 'NONE', #10929, 1000.000000000000000 ) ;
#3353 = ORIENTED_EDGE ( 'NONE', *, *, #10094, .F. ) ;
#3354 = DIRECTION ( 'NONE',  ( -0.08715574274764828488, -0.4980973490458772135, 0.8627299156628193133 ) ) ;
#3355 = AXIS2_PLACEMENT_3D ( 'NONE', #167, #5574, #4426 ) ;
#3356 = ORIENTED_EDGE ( 'NONE', *, *, #7036, .F. ) ;
#3357 = DIRECTION ( 'NONE',  ( 1.000000000000000000, -0.000000000000000000, -0.000000000000000000 ) ) ;
#3358 = CARTESIAN_POINT ( 'NONE',  ( 32.99999999999998579, 9.999999999999998224, -35.00200000000000244 ) ) ;
#3359 = EDGE_CURVE ( 'NONE', #13584, #5251, #5104, .T. ) ;
#3360 = CARTESIAN_POINT ( 'NONE',  ( -70.00000000000000000, 171.6227766016838245, 20.00000000000000355 ) ) ;
#3361 = ORIENTED_EDGE ( 'NONE', *, *, #13937, .T. ) ;
#3362 = LINE ( 'NONE', #12825, #3312 ) ;
#3363 = DIRECTION ( 'NONE',  ( -0.000000000000000000, -0.000000000000000000, -1.000000000000000000 ) ) ;
#3364 = VECTOR ( 'NONE', #12098, 1000.000000000000000 ) ;
#3365 = CARTESIAN_POINT ( 'NONE',  ( -73.00000000000001421, 171.6227766016838245, 0.000000000000000000 ) ) ;
#3366 = VECTOR ( 'NONE', #15734, 1000.000000000000000 ) ;
#3367 = CARTESIAN_POINT ( 'NONE',  ( 30.93864055801722657, 202.5503328113395014, -16.38559373769485461 ) ) ;
#3368 = VERTEX_POINT ( 'NONE', #1466 ) ;
#3369 = ORIENTED_EDGE ( 'NONE', *, *, #4116, .F. ) ;
#3370 = CARTESIAN_POINT ( 'NONE',  ( 27.13959012325755538, 19.99999999999999645, -20.89788123228700556 ) ) ;
#3371 = CARTESIAN_POINT ( 'NONE',  ( -207.6513770290094669, 170.7478318238843542, 4.898587196589412829E-16 ) ) ;
#3372 = EDGE_LOOP ( 'NONE', ( #6101, #11259 ) ) ;
#3373 = CIRCLE ( 'NONE', #12402, 30.00000000000000000 ) ;
#3374 = DIRECTION ( 'NONE',  ( 1.000000000000000000, -0.000000000000000000, -0.000000000000000000 ) ) ;
#3375 = DIRECTION ( 'NONE',  ( -1.000000000000000000, 0.000000000000000000, 0.000000000000000000 ) ) ;
#3376 = EDGE_LOOP ( 'NONE', ( #6301, #7871, #10654, #1627, #10607 ) ) ;
#3377 = CIRCLE ( 'NONE', #6186, 5.000000000000006217 ) ;
#3378 = DIRECTION ( 'NONE',  ( -1.000000000000000000, -0.000000000000000000, -0.000000000000000000 ) ) ;
#3379 = CIRCLE ( 'NONE', #2808, 2.499999999999998668 ) ;
#3380 = ADVANCED_FACE ( 'NONE', ( #9502 ), #6782, .F. ) ;
#3381 = CYLINDRICAL_SURFACE ( 'NONE', #4941, 6.000000000000001776 ) ;
#3382 = CARTESIAN_POINT ( 'NONE',  ( -19.26597175465492739, 18.00000000000000000, 21.35691006828201566 ) ) ;
#3383 = DIRECTION ( 'NONE',  ( -1.000000000000000000, -0.000000000000000000, -0.000000000000000000 ) ) ;
#3384 = CARTESIAN_POINT ( 'NONE',  ( -48.00000000000000000, 171.6227766016838245, 0.000000000000000000 ) ) ;
#3385 = VERTEX_POINT ( 'NONE', #9676 ) ;
#3386 = CARTESIAN_POINT ( 'NONE',  ( 17.00000000000000000, 154.3022685259950038, -9.999999999999900524 ) ) ;
#3387 = CIRCLE ( 'NONE', #9873, 5.000000000000000888 ) ;
#3388 = EDGE_CURVE ( 'NONE', #16699, #10429, #1147, .T. ) ;
#3389 = B_SPLINE_CURVE_WITH_KNOTS ( 'NONE', 3,
 ( #16697, #12527, #1733, #15352 ),
 .UNSPECIFIED., .F., .F.,
 ( 4, 4 ),
 ( 0.000000000000000000, 0.003672568685860802366 ),
 .UNSPECIFIED. ) ;
#3390 = ORIENTED_EDGE ( 'NONE', *, *, #14733, .F. ) ;
#3391 = EDGE_CURVE ( 'NONE', #15051, #13756, #14704, .T. ) ;
#3392 = CARTESIAN_POINT ( 'NONE',  ( 39.99999999999998579, 20.00000000000000000, 30.00000000000001066 ) ) ;
#3393 = CIRCLE ( 'NONE', #9880, 2.500000000000002220 ) ;
#3394 = EDGE_CURVE ( 'NONE', #2136, #9101, #14996, .T. ) ;
#3395 = LINE ( 'NONE', #4550, #7517 ) ;
#3396 = ORIENTED_EDGE ( 'NONE', *, *, #1958, .T. ) ;
#3397 = CYLINDRICAL_SURFACE ( 'NONE', #698, 10.00000000000000000 ) ;
#3398 = CARTESIAN_POINT ( 'NONE',  ( -74.40238044657790795, 201.6350306476045091, -13.74486639216964079 ) ) ;
#3399 = CARTESIAN_POINT ( 'NONE',  ( 14.92319712166297840, 137.6313713749984800, 10.11910373048645440 ) ) ;
#3400 = AXIS2_PLACEMENT_3D ( 'NONE', #13612, #12192, #9431 ) ;
#3401 = VECTOR ( 'NONE', #13375, 1000.000000000000000 ) ;
#3402 = ORIENTED_EDGE ( 'NONE', *, *, #16848, .F. ) ;
#3403 = ITEM_DEFINED_TRANSFORMATION ( 'NONE', 'NONE', #505,  #3583 ) ;
#3404 = LINE ( 'NONE', #12602, #7236 ) ;
#3405 = CARTESIAN_POINT ( 'NONE',  ( -75.16864359540511487, 195.3043783022527862, 22.98536326679098707 ) ) ;
#3406 = CARTESIAN_POINT ( 'NONE',  ( -11.99846793330598693, 31.02137248309377071, -14.08482506821421509 ) ) ;
#3407 = CYLINDRICAL_SURFACE ( 'NONE', #14893, 19.49999999999998934 ) ;
#3408 = DIRECTION ( 'NONE',  ( 1.000000000000000000, -0.000000000000000000, -0.000000000000000000 ) ) ;
#3409 = ORIENTED_EDGE ( 'NONE', *, *, #8607, .T. ) ;
#3410 = CARTESIAN_POINT ( 'NONE',  ( 30.00000000000000355, 196.6227766016838245, -13.00000000000000000 ) ) ;
#3411 = CARTESIAN_POINT ( 'NONE',  ( -27.98221281347037959, 20.00000000000000000, -4.999999999999999112 ) ) ;
#3412 = ORIENTED_EDGE ( 'NONE', *, *, #7648, .T. ) ;
#3413 = CARTESIAN_POINT ( 'NONE',  ( 48.00000000000000711, 155.6227766016839098, 12.50000337241049309 ) ) ;
#3414 = DIRECTION ( 'NONE',  ( -1.000000000000000000, 0.000000000000000000, 0.000000000000000000 ) ) ;
#3415 = AXIS2_PLACEMENT_3D ( 'NONE', #2819, #10786, #9276 ) ;
#3416 = VERTEX_POINT ( 'NONE', #5447 ) ;
#3417 = ORIENTED_EDGE ( 'NONE', *, *, #6319, .T. ) ;
#3418 = AXIS2_PLACEMENT_3D ( 'NONE', #1376, #218, #13410 ) ;
#3419 = VERTEX_POINT ( 'NONE', #1637 ) ;
#3420 = DIRECTION ( 'NONE',  ( 1.000000000000000000, 0.000000000000000000, 0.000000000000000000 ) ) ;
#3421 = VERTEX_POINT ( 'NONE', #14912 ) ;
#3422 = EDGE_CURVE ( 'NONE', #12595, #8077, #4266, .T. ) ;
#3423 = ADVANCED_FACE ( 'NONE', ( #5710, #10918 ), #308, .F. ) ;
#3424 = DIRECTION ( 'NONE',  ( 0.000000000000000000, 0.000000000000000000, 1.000000000000000000 ) ) ;
#3425 = DIRECTION ( 'NONE',  ( 0.000000000000000000, 0.000000000000000000, -1.000000000000000000 ) ) ;
#3426 = SPHERICAL_SURFACE ( 'NONE', #12135, 5.315148208181398104 ) ;
#3427 = CIRCLE ( 'NONE', #13321, 20.00000000000000355 ) ;
#3428 = DIRECTION ( 'NONE',  ( 0.000000000000000000, 0.000000000000000000, 1.000000000000000000 ) ) ;
#3429 = ORIENTED_EDGE ( 'NONE', *, *, #2022, .T. ) ;
#3430 = CARTESIAN_POINT ( 'NONE',  ( 27.50000000000000355, 196.6227766016838245, 10.00000000000000178 ) ) ;
#3431 = LINE ( 'NONE', #2016, #6489 ) ;
#3432 = DIRECTION ( 'NONE',  ( -1.000000000000000000, -0.000000000000000000, -0.000000000000000000 ) ) ;
#3433 = CARTESIAN_POINT ( 'NONE',  ( -14.51002702888200702, 31.55035369552022928, -12.57309263104575869 ) ) ;
#3434 = CARTESIAN_POINT ( 'NONE',  ( 27.99999999999998224, 9.999999999999998224, -12.99999999999999822 ) ) ;
#3435 = AXIS2_PLACEMENT_3D ( 'NONE', #1263, #10821, #5163 ) ;
#3436 = DIRECTION ( 'NONE',  ( -1.000000000000000000, 0.000000000000000000, 0.000000000000000000 ) ) ;
#3437 = ORIENTED_EDGE ( 'NONE', *, *, #13167, .F. ) ;
#3438 = DIRECTION ( 'NONE',  ( -1.000000000000000000, 0.000000000000000000, 0.000000000000000000 ) ) ;
#3439 = ORIENTED_EDGE ( 'NONE', *, *, #3790, .T. ) ;
#3440 = EDGE_CURVE ( 'NONE', #15255, #3416, #7650, .T. ) ;
#3441 = SURFACE_SIDE_STYLE ('',( #15381 ) ) ;
#3442 = ADVANCED_FACE ( 'NONE', ( #9595 ), #14998, .T. ) ;
#3443 = LINE ( 'NONE', #14238, #11031 ) ;
#3444 = EDGE_CURVE ( 'NONE', #7056, #1055, #3996, .T. ) ;
#3445 = EDGE_CURVE ( 'NONE', #1301, #9322, #13675, .T. ) ;
#3446 = CARTESIAN_POINT ( 'NONE',  ( 27.99999999999998224, 9.999999999999998224, 0.000000000000000000 ) ) ;
#3447 = CARTESIAN_POINT ( 'NONE',  ( 6.134011831684049731, 134.2062027339443944, -13.00000000000000000 ) ) ;
#3448 = ORIENTED_EDGE ( 'NONE', *, *, #4810, .F. ) ;
#3449 = PLANE ( 'NONE',  #15184 ) ;
#3450 = FACE_OUTER_BOUND ( 'NONE', #8697, .T. ) ;
#3451 = DIRECTION ( 'NONE',  ( 1.000000000000000000, -0.000000000000000000, -0.000000000000000000 ) ) ;
#3452 = CARTESIAN_POINT ( 'NONE',  ( 24.26110014372655144, 198.4077499201236776, -22.53509453904542070 ) ) ;
#3453 = ORIENTED_EDGE ( 'NONE', *, *, #12739, .T. ) ;
#3454 = VERTEX_POINT ( 'NONE', #10758 ) ;
#3455 = CARTESIAN_POINT ( 'NONE',  ( 28.14717441101472772, 19.99999999999999645, -20.07001214883818108 ) ) ;
#3456 = DIRECTION ( 'NONE',  ( 1.000000000000000000, 0.000000000000000000, 0.000000000000000000 ) ) ;
#3457 = ORIENTED_EDGE ( 'NONE', *, *, #4306, .T. ) ;
#3458 = ADVANCED_FACE ( 'NONE', ( #6049 ), #4378, .F. ) ;
#3459 = FACE_OUTER_BOUND ( 'NONE', #12755, .T. ) ;
#3460 = DIRECTION ( 'NONE',  ( -1.000000000000000000, 0.000000000000000000, 0.000000000000000000 ) ) ;
#3461 = ORIENTED_EDGE ( 'NONE', *, *, #15421, .T. ) ;
#3462 = DIRECTION ( 'NONE',  ( 1.000000000000000000, 0.000000000000000000, -0.000000000000000000 ) ) ;
#3463 = UNCERTAINTY_MEASURE_WITH_UNIT (LENGTH_MEASURE( 1.000000000000000082E-05 ), #1037, 'distance_accuracy_value', 'NONE');
#3464 = DIRECTION ( 'NONE',  ( 6.938893903907229364E-16, -3.469446951953614682E-16, -1.000000000000000000 ) ) ;
#3465 = DIRECTION ( 'NONE',  ( 1.000000000000000000, 0.000000000000000000, 0.000000000000000000 ) ) ;
#3466 = CARTESIAN_POINT ( 'NONE',  ( -16.24840885328083928, 32.75254598042347709, 6.058899415740283345 ) ) ;
#3467 = DIRECTION ( 'NONE',  ( 0.000000000000000000, 0.000000000000000000, 1.000000000000000000 ) ) ;
#3468 = CYLINDRICAL_SURFACE ( 'NONE', #14273, 5.999999999999998224 ) ;
#3469 = ORIENTED_EDGE ( 'NONE', *, *, #15762, .T. ) ;
#3470 = CARTESIAN_POINT ( 'NONE',  ( 6.134011831684053284, 142.5209969267753820, -19.44444444444444642 ) ) ;
#3471 = ORIENTED_EDGE ( 'NONE', *, *, #11776, .T. ) ;
#3472 = DIRECTION ( 'NONE',  ( -0.000000000000000000, -0.000000000000000000, 1.000000000000000000 ) ) ;
#3473 = CARTESIAN_POINT ( 'NONE',  ( -32.66708739526796279, 118.9256726598784866, 4.648823768412006174 ) ) ;
#3474 = ADVANCED_FACE ( 'NONE', ( #5973 ), #7199, .F. ) ;
#3475 = VERTEX_POINT ( 'NONE', #11444 ) ;
#3476 = ADVANCED_FACE ( 'NONE', ( #11180 ), #16854, .F. ) ;
#3477 = DIRECTION ( 'NONE',  ( 1.000000000000000000, -0.000000000000000000, -2.312964634635742957E-16 ) ) ;
#3478 = EDGE_CURVE ( 'NONE', #3840, #8790, #11607, .T. ) ;
#3479 = CARTESIAN_POINT ( 'NONE',  ( 24.93034343272635667, 19.99999999999999645, 22.33460256652156062 ) ) ;
#3480 = ORIENTED_EDGE ( 'NONE', *, *, #10562, .F. ) ;
#3481 = EDGE_CURVE ( 'NONE', #2477, #9250, #7696, .T. ) ;
#3482 = DIRECTION ( 'NONE',  ( 0.000000000000000000, 0.000000000000000000, 1.000000000000000000 ) ) ;
#3483 = EDGE_CURVE ( 'NONE', #11751, #10197, #9915, .T. ) ;
#3484 = CARTESIAN_POINT ( 'NONE',  ( -76.23821662194384885, 193.3250171236886104, 24.86042266551077873 ) ) ;
#3485 = CARTESIAN_POINT ( 'NONE',  ( -14.33532356861720380, 31.51408589783374126, -12.70909354450696149 ) ) ;
#3486 = LINE ( 'NONE', #10621, #5572 ) ;
#3487 = DIRECTION ( 'NONE',  ( -1.000000000000000000, -0.000000000000000000, -0.000000000000000000 ) ) ;
#3488 = ORIENTED_EDGE ( 'NONE', *, *, #13115, .F. ) ;
#3489 = DIRECTION ( 'NONE',  ( 1.000000000000000000, 0.000000000000000000, 0.000000000000000000 ) ) ;
#3490 = DIRECTION ( 'NONE',  ( 1.000000000000000000, 0.000000000000000000, 0.000000000000000000 ) ) ;
#3491 = EDGE_LOOP ( 'NONE', ( #4673, #7484, #5566, #8858, #5429, #6779, #9966 ) ) ;
#3492 = CARTESIAN_POINT ( 'NONE',  ( 25.97411924848963594, 192.1541050315147459, -28.34722919022666332 ) ) ;
#3493 = FACE_BOUND ( 'NONE', #6892, .T. ) ;
#3494 = ORIENTED_EDGE ( 'NONE', *, *, #12359, .F. ) ;
#3495 = ORIENTED_EDGE ( 'NONE', *, *, #5514, .F. ) ;
#3496 = EDGE_LOOP ( 'NONE', ( #8699, #3235, #10892, #16646, #7400, #1142, #6745, #10375, #12379, #5360 ) ) ;
#3497 = ORIENTED_EDGE ( 'NONE', *, *, #3823, .T. ) ;
#3498 = CARTESIAN_POINT ( 'NONE',  ( -87.49298393897305459, 147.0010062438373950, -21.97388680505723002 ) ) ;
#3499 = EDGE_LOOP ( 'NONE', ( #17074, #5080, #669, #10368, #13006 ) ) ;
#3500 =( NAMED_UNIT ( * ) PLANE_ANGLE_UNIT ( ) SI_UNIT ( $, .RADIAN. ) );
#3501 = DIRECTION ( 'NONE',  ( 8.673617379884037937E-17, 0.000000000000000000, 1.000000000000000000 ) ) ;
#3502 = CARTESIAN_POINT ( 'NONE',  ( 14.79728876016037198, 126.7368160533725643, 7.941237055946955614 ) ) ;
#3503 = EDGE_CURVE ( 'NONE', #11327, #8547, #13862, .T. ) ;
#3504 = PLANE ( 'NONE',  #14956 ) ;
#3505 = CARTESIAN_POINT ( 'NONE',  ( 20.85766706164172035, 17.99999999999999645, 10.55326734450395954 ) ) ;
#3506 = CARTESIAN_POINT ( 'NONE',  ( -100.0000000000000000, 141.6227766016838245, 0.000000000000000000 ) ) ;
#3507 = AXIS2_PLACEMENT_3D ( 'NONE', #16272, #16001, #1308 ) ;
#3508 = ORIENTED_EDGE ( 'NONE', *, *, #3478, .T. ) ;
#3509 = PLANE ( 'NONE',  #13524 ) ;
#3510 = CARTESIAN_POINT ( 'NONE',  ( -27.99999999999998224, 10.00000000000000000, -13.00000000000000000 ) ) ;
#3511 = CARTESIAN_POINT ( 'NONE',  ( 49.99999999999998579, 151.6227766016839098, -3.071800142134974099 ) ) ;
#3512 = CARTESIAN_POINT ( 'NONE',  ( 23.92262868871285519, 29.88142130320016676, 9.432657661123421633 ) ) ;
#3513 = CARTESIAN_POINT ( 'NONE',  ( 2.426025403784448642, 0.000000000000000000, 2.168404344971008868E-16 ) ) ;
#3514 = EDGE_CURVE ( 'NONE', #11646, #8664, #8503, .T. ) ;
#3515 = CARTESIAN_POINT ( 'NONE',  ( 32.22224914908579763, 201.1051302811612516, 14.82644580554060987 ) ) ;
#3516 = ORIENTED_EDGE ( 'NONE', *, *, #3445, .T. ) ;
#3517 = DIRECTION ( 'NONE',  ( 0.000000000000000000, 0.000000000000000000, -1.000000000000000000 ) ) ;
#3518 = CARTESIAN_POINT ( 'NONE',  ( -32.66708739526796279, 119.0000000000000284, 5.500000000000000000 ) ) ;
#3519 = VECTOR ( 'NONE', #11349, 1000.000000000000000 ) ;
#3520 = ORIENTED_EDGE ( 'NONE', *, *, #10861, .F. ) ;
#3521 = CARTESIAN_POINT ( 'NONE',  ( 196.0000000000000000, 155.6227766016839098, 10.00000337241049309 ) ) ;
#3522 = AXIS2_PLACEMENT_3D ( 'NONE', #9734, #5760, #3014 ) ;
#3523 = DIRECTION ( 'NONE',  ( 0.000000000000000000, -1.000000000000000000, 0.000000000000000000 ) ) ;
#3524 = CARTESIAN_POINT ( 'NONE',  ( 48.00000000000000711, 175.6227766016838530, 19.42820660268601074 ) ) ;
#3525 = ORIENTED_EDGE ( 'NONE', *, *, #9081, .T. ) ;
#3526 = LINE ( 'NONE', #3785, #12093 ) ;
#3527 = FACE_OUTER_BOUND ( 'NONE', #12622, .T. ) ;
#3528 = CARTESIAN_POINT ( 'NONE',  ( 48.00000000000000711, 179.6227766016838245, 12.50000337241049309 ) ) ;
#3529 = CARTESIAN_POINT ( 'NONE',  ( 34.07337191958318101, 201.0442424278814428, -18.96251499051322753 ) ) ;
#3530 = VECTOR ( 'NONE', #14519, 1000.000000000000000 ) ;
#3531 = EDGE_LOOP ( 'NONE', ( #16082, #13773 ) ) ;
#3532 = EDGE_CURVE ( 'NONE', #4990, #6914, #15292, .T. ) ;
#3533 = ADVANCED_FACE ( 'NONE', ( #13102 ), #15757, .F. ) ;
#3534 = CIRCLE ( 'NONE', #4099, 2.500000000000002220 ) ;
#3535 = ADVANCED_FACE ( 'NONE', ( #3219 ), #1804, .T. ) ;
#3536 = ORIENTED_EDGE ( 'NONE', *, *, #3394, .F. ) ;
#3537 = CARTESIAN_POINT ( 'NONE',  ( 19.35452547490215736, 29.94096051140668280, -13.97567760708249551 ) ) ;
#3538 = EDGE_CURVE ( 'NONE', #9695, #17286, #12519, .T. ) ;
#3539 = EDGE_CURVE ( 'NONE', #6279, #209, #7013, .T. ) ;
#3540 = CARTESIAN_POINT ( 'NONE',  ( -75.00000000000000000, 196.6227766016838245, 21.54065922853802206 ) ) ;
#3541 = ORIENTED_EDGE ( 'NONE', *, *, #11525, .T. ) ;
#3542 = CYLINDRICAL_SURFACE ( 'NONE', #11779, 2.500000000000000444 ) ;
#3543 = DIRECTION ( 'NONE',  ( 1.000000000000000000, 0.000000000000000000, 8.673617379884037937E-17 ) ) ;
#3544 = ORIENTED_EDGE ( 'NONE', *, *, #8827, .F. ) ;
#3545 = DIRECTION ( 'NONE',  ( 0.000000000000000000, 1.000000000000000000, 1.224646799147353207E-16 ) ) ;
#3546 = STYLED_ITEM ( 'NONE', ( #13619 ), #5314 ) ;
#3547 = CIRCLE ( 'NONE', #2407, 6.000000000000005329 ) ;
#3548 = CARTESIAN_POINT ( 'NONE',  ( -40.00000000000000000, 20.00000000000000000, 0.000000000000000000 ) ) ;
#3549 = CARTESIAN_POINT ( 'NONE',  ( -95.00000000000000000, 143.9321776784423150, 5.086680500673126297E-15 ) ) ;
#3550 = CARTESIAN_POINT ( 'NONE',  ( -10.22933296213221865, 30.92590585860461161, 12.59260918105267457 ) ) ;
#3551 = CARTESIAN_POINT ( 'NONE',  ( -15.00000000000001421, 130.0000000000000000, 13.00000000000000000 ) ) ;
#3552 = DIRECTION ( 'NONE',  ( 0.000000000000000000, 1.040834085586084059E-15, -1.000000000000000000 ) ) ;
#3553 = ORIENTED_EDGE ( 'NONE', *, *, #14370, .T. ) ;
#3554 = DIRECTION ( 'NONE',  ( -0.000000000000000000, -0.000000000000000000, -1.000000000000000000 ) ) ;
#3555 = ORIENTED_EDGE ( 'NONE', *, *, #6625, .T. ) ;
#3556 = LINE ( 'NONE', #2056, #6781 ) ;
#3557 = EDGE_CURVE ( 'NONE', #13930, #11460, #471, .T. ) ;
#3558 = AXIS2_PLACEMENT_3D ( 'NONE', #17490, #9597, #16342 ) ;
#3559 = CARTESIAN_POINT ( 'NONE',  ( -100.0000000000000000, 171.6227766016838245, 0.000000000000000000 ) ) ;
#3560 = TOROIDAL_SURFACE ( 'NONE', #10616, 21.61734737250326077, 2.000000000000000000 ) ;
#3561 = EDGE_LOOP ( 'NONE', ( #966, #7996, #9790, #1341 ) ) ;
#3562 = CARTESIAN_POINT ( 'NONE',  ( -153.0000000000000284, 171.6227766016838245, 0.000000000000000000 ) ) ;
#3563 = CARTESIAN_POINT ( 'NONE',  ( 34.80444759362561058, 19.99999999999999645, 7.621511755370173447 ) ) ;
#3564 = EDGE_LOOP ( 'NONE', ( #3924, #13589, #644, #3850 ) ) ;
#3565 = DIRECTION ( 'NONE',  ( 0.000000000000000000, 0.000000000000000000, 1.000000000000000000 ) ) ;
#3566 = AXIS2_PLACEMENT_3D ( 'NONE', #7634, #16053, #17105 ) ;
#3567 = CARTESIAN_POINT ( 'NONE',  ( 23.52759457847468383, 192.8264746069455100, -25.28784208911849518 ) ) ;
#3568 = CARTESIAN_POINT ( 'NONE',  ( -16.66926302330761800, 31.99181794709938487, -10.22419352058821396 ) ) ;
#3569 = AXIS2_PLACEMENT_3D ( 'NONE', #11001, #13667, #12332 ) ;
#3570 = CARTESIAN_POINT ( 'NONE',  ( -9.245637070518823109, 17.99999999999769074, -12.12237611798427572 ) ) ;
#3571 = EDGE_CURVE ( 'NONE', #4864, #12384, #6166, .T. ) ;
#3572 = ORIENTED_EDGE ( 'NONE', *, *, #11370, .F. ) ;
#3573 = CARTESIAN_POINT ( 'NONE',  ( 48.00000000000000000, 171.6227766016838245, 12.50000337241049131 ) ) ;
#3574 = CARTESIAN_POINT ( 'NONE',  ( -26.89314795393037016, 19.99999999999999289, -11.55702759004480207 ) ) ;
#3575 = ORIENTED_EDGE ( 'NONE', *, *, #4203, .F. ) ;
#3576 = CARTESIAN_POINT ( 'NONE',  ( -22.93725393319379791, 120.0000000000000284, -6.000000000000001776 ) ) ;
#3577 = CARTESIAN_POINT ( 'NONE',  ( -22.93725393319379435, 100.0000000000000142, 6.000000000000000000 ) ) ;
#3578 = ORIENTED_EDGE ( 'NONE', *, *, #17229, .T. ) ;
#3579 = ORIENTED_EDGE ( 'NONE', *, *, #11915, .T. ) ;
#3580 = EDGE_LOOP ( 'NONE', ( #10134, #10364, #5963, #94 ) ) ;
#3581 = VECTOR ( 'NONE', #11685, 1000.000000000000000 ) ;
#3582 = AXIS2_PLACEMENT_3D ( 'NONE', #6896, #1684, #87 ) ;
#3584 = CARTESIAN_POINT ( 'NONE',  ( -77.99239453806532651, 153.8546784850604183, -27.80828541846620539 ) ) ;
#3583 = AXIS2_PLACEMENT_3D ( 'NONE', #5482, #6893, #8222 ) ;
#3585 = VECTOR ( 'NONE', #8683, 1000.000000000000000 ) ;
#3586 = ORIENTED_EDGE ( 'NONE', *, *, #13440, .T. ) ;
#3587 = CARTESIAN_POINT ( 'NONE',  ( -80.00000000000002842, 146.6227766016838245, -18.75000000000000355 ) ) ;
#3588 = CARTESIAN_POINT ( 'NONE',  ( -11.09520285051611488, 31.19962993084977398, 12.30130330100619673 ) ) ;
#3589 = CARTESIAN_POINT ( 'NONE',  ( -16.47274440071381107, 31.95215739789422571, 10.50982007662407725 ) ) ;
#3590 = CARTESIAN_POINT ( 'NONE',  ( 27.18872211705360087, 151.9278302392748685, -28.93306197017448866 ) ) ;
#3591 = DIRECTION ( 'NONE',  ( -8.673617379884037937E-17, 0.000000000000000000, 1.000000000000000000 ) ) ;
#3592 = DIRECTION ( 'NONE',  ( 0.000000000000000000, 1.000000000000000000, 0.000000000000000000 ) ) ;
#3593 = EDGE_CURVE ( 'NONE', #13962, #6224, #14439, .T. ) ;
#3594 = ORIENTED_EDGE ( 'NONE', *, *, #2938, .T. ) ;
#3595 = CARTESIAN_POINT ( 'NONE',  ( -167.6513770290094385, 170.3104757200652273, -2.272971801780872880 ) ) ;
#3596 = FACE_OUTER_BOUND ( 'NONE', #10262, .T. ) ;
#3597 = CIRCLE ( 'NONE', #14907, 10.00000000000000000 ) ;
#3598 = CARTESIAN_POINT ( 'NONE',  ( 17.54349574104648823, 125.4948194589026684, 4.999999999999997335 ) ) ;
#3599 = CARTESIAN_POINT ( 'NONE',  ( -27.30244652380281778, 19.99999999999999645, -10.27378278477019080 ) ) ;
#3600 = EDGE_LOOP ( 'NONE', ( #5876, #108, #270, #2076, #17078, #12969, #15156, #1622, #10911, #3632, #10206, #13256, #7640, #16853, #15534, #14751, #17072, #1127, #2160, #16582, #4030, #16067, #12740, #15190, #14548, #13523, #13112, #16327, #15322, #9084, #8366, #16483, #1114, #13916, #11093, #10413, #17185, #1539, #16241, #14464, #5400, #11636, #10826, #13850, #3048, #3145, #12610, #913, #1568, #12722, #5229, #6318, #12758, #5147, #17153 ) ) ;
#3601 = DIRECTION ( 'NONE',  ( 1.000000000000000000, -0.000000000000000000, -0.000000000000000000 ) ) ;
#3602 = ADVANCED_FACE ( 'NONE', ( #3311 ), #13526, .F. ) ;
#3603 =( REPRESENTATION_RELATIONSHIP ('NONE','NONE', #9723, #6585 ) REPRESENTATION_RELATIONSHIP_WITH_TRANSFORMATION ( #8532 )SHAPE_REPRESENTATION_RELATIONSHIP( ) );
#3604 = ADVANCED_FACE ( 'NONE', ( #11764, #13191 ), #4001, .F. ) ;
#3605 = EDGE_CURVE ( 'NONE', #1036, #16730, #8421, .T. ) ;
#3606 = CARTESIAN_POINT ( 'NONE',  ( 27.03183975455296917, 200.6580771142793083, 15.68801935549129745 ) ) ;
#3607 = ORIENTED_EDGE ( 'NONE', *, *, #11009, .T. ) ;
#3608 = FACE_OUTER_BOUND ( 'NONE', #4104, .T. ) ;
#3609 = DIRECTION ( 'NONE',  ( 0.000000000000000000, -1.000000000000000000, 0.000000000000000000 ) ) ;
#3610 = VERTEX_POINT ( 'NONE', #7874 ) ;
#3611 = DIRECTION ( 'NONE',  ( -1.000000000000000000, 0.000000000000000000, 0.000000000000000000 ) ) ;
#3612 = CARTESIAN_POINT ( 'NONE',  ( -151.0000000000000284, 171.6227766016838245, 23.57392898041431195 ) ) ;
#3613 = CIRCLE ( 'NONE', #16354, 6.000000000000001776 ) ;
#3614 = CARTESIAN_POINT ( 'NONE',  ( 17.00458606767794834, 29.95830270928036398, -12.72829919683579902 ) ) ;
#3615 = CARTESIAN_POINT ( 'NONE',  ( -48.00000000000000000, 171.6227766016838245, 0.000000000000000000 ) ) ;
#3616 = EDGE_CURVE ( 'NONE', #4595, #9313, #8986, .T. ) ;
#3617 = CARTESIAN_POINT ( 'NONE',  ( 9.186438336152177087, 132.7758989760081931, -12.51111164240594675 ) ) ;
#3618 = ORIENTED_EDGE ( 'NONE', *, *, #12145, .T. ) ;
#3619 = LINE ( 'NONE', #5122, #7835 ) ;
#3620 = CARTESIAN_POINT ( 'NONE',  ( -90.80384757729339640, 204.6227766016838245, 0.000000000000000000 ) ) ;
#3621 = CARTESIAN_POINT ( 'NONE',  ( 48.00000000000000711, 159.6227766016838814, 8.071800142134975431 ) ) ;
#3622 = CARTESIAN_POINT ( 'NONE',  ( 24.65540802277405064, 199.3716779298525239, -21.33657927093678452 ) ) ;
#3623 = ORIENTED_EDGE ( 'NONE', *, *, #8513, .T. ) ;
#3624 = ORIENTED_EDGE ( 'NONE', *, *, #16804, .T. ) ;
#3625 = CARTESIAN_POINT ( 'NONE',  ( 15.58467296311467898, 20.00000000001131895, -15.00881168888636807 ) ) ;
#3626 = AXIS2_PLACEMENT_3D ( 'NONE', #13286, #1236, #2383 ) ;
#3627 =( GEOMETRIC_REPRESENTATION_CONTEXT ( 3 ) GLOBAL_UNCERTAINTY_ASSIGNED_CONTEXT ( ( #14095 ) ) GLOBAL_UNIT_ASSIGNED_CONTEXT ( ( #11921, #2552, #17326 ) ) REPRESENTATION_CONTEXT ( 'NONE', 'WORKASPACE' ) );
#3628 = CARTESIAN_POINT ( 'NONE',  ( 10.98422133653362920, 132.2143956889292724, -13.95899527751216240 ) ) ;
#3629 = VERTEX_POINT ( 'NONE', #4075 ) ;
#3630 = DIRECTION ( 'NONE',  ( 1.000000000000000000, 0.000000000000000000, 0.000000000000000000 ) ) ;
#3631 = CARTESIAN_POINT ( 'NONE',  ( 13.54862175821475034, 128.4555333983033734, -9.713103375557215813 ) ) ;
#3632 = ORIENTED_EDGE ( 'NONE', *, *, #16739, .F. ) ;
#3633 = DIRECTION ( 'NONE',  ( 0.000000000000000000, 0.000000000000000000, -1.000000000000000000 ) ) ;
#3634 = DIRECTION ( 'NONE',  ( 0.000000000000000000, 1.000000000000000000, 0.000000000000000000 ) ) ;
#3635 = EDGE_CURVE ( 'NONE', #11591, #13399, #17474, .T. ) ;
#3636 = ADVANCED_FACE ( 'NONE', ( #2479 ), #13231, .T. ) ;
#3637 = VECTOR ( 'NONE', #16218, 1000.000000000000114 ) ;
#3638 = EDGE_CURVE ( 'NONE', #6756, #5589, #5219, .T. ) ;
#3639 = CIRCLE ( 'NONE', #13537, 19.49999999999998224 ) ;
#3640 = LINE ( 'NONE', #2216, #3874 ) ;
#3641 = CARTESIAN_POINT ( 'NONE',  ( -100.0000000000000000, 171.6227766016838245, 30.00000000000000711 ) ) ;
#3642 = CARTESIAN_POINT ( 'NONE',  ( -12.22383789047832181, 18.00000000000231992, 8.612907111650555336 ) ) ;
#3643 = CARTESIAN_POINT ( 'NONE',  ( -23.00000000000002132, 122.0000000000000142, 9.686291501015228178 ) ) ;
#3644 = CARTESIAN_POINT ( 'NONE',  ( 14.93242934743711992, 30.00000000000000000, -25.00000000000000000 ) ) ;
#3645 = EDGE_LOOP ( 'NONE', ( #587, #13764, #622, #8083 ) ) ;
#3646 = DIRECTION ( 'NONE',  ( 0.000000000000000000, 0.000000000000000000, 1.000000000000000000 ) ) ;
#3647 = ORIENTED_EDGE ( 'NONE', *, *, #11674, .F. ) ;
#3648 = DIRECTION ( 'NONE',  ( 1.000000000000000000, 0.000000000000000000, 0.000000000000000000 ) ) ;
#3649 = AXIS2_PLACEMENT_3D ( 'NONE', #955, #6350, #11745 ) ;
#3650 = DIRECTION ( 'NONE',  ( 0.000000000000000000, 0.000000000000000000, 1.000000000000000000 ) ) ;
#3651 = AXIS2_PLACEMENT_3D ( 'NONE', #10106, #8603, #12684 ) ;
#3652 = ORIENTED_EDGE ( 'NONE', *, *, #5137, .T. ) ;
#3653 = CARTESIAN_POINT ( 'NONE',  ( 14.93242934743711992, 20.00000000000000000, 25.00000000000000000 ) ) ;
#3654 = AXIS2_PLACEMENT_3D ( 'NONE', #990, #2240, #13312 ) ;
#3655 = FACE_OUTER_BOUND ( 'NONE', #11920, .T. ) ;
#3656 = CARTESIAN_POINT ( 'NONE',  ( -73.57895800238922845, 200.5259344270104691, -15.94638436093396372 ) ) ;
#3657 = EDGE_LOOP ( 'NONE', ( #4900, #6020, #8332, #11775 ) ) ;
#3658 = EDGE_CURVE ( 'NONE', #2441, #5035, #9555, .T. ) ;
#3659 = ADVANCED_FACE ( 'NONE', ( #10441 ), #8137, .F. ) ;
#3660 = CARTESIAN_POINT ( 'NONE',  ( -725.0000000000000000, 19.99999999999995737, -4.999999999999999112 ) ) ;
#3661 = LINE ( 'NONE', #7635, #5918 ) ;
#3662 = CIRCLE ( 'NONE', #1122, 2.699999999999999289 ) ;
#3663 = VECTOR ( 'NONE', #7410, 1000.000000000000000 ) ;
#3664 = DIRECTION ( 'NONE',  ( 1.000000000000000000, 0.000000000000000000, -0.000000000000000000 ) ) ;
#3665 = VECTOR ( 'NONE', #5233, 1000.000000000000000 ) ;
#3666 = CARTESIAN_POINT ( 'NONE',  ( -12.80328004466210601, 18.00000000000000000, -4.999999999999999112 ) ) ;
#3667 = AXIS2_PLACEMENT_3D ( 'NONE', #8932, #14257, #10184 ) ;
#3668 = ORIENTED_EDGE ( 'NONE', *, *, #4719, .T. ) ;
#3669 = LINE ( 'NONE', #9057, #16907 ) ;
#3670 = EDGE_LOOP ( 'NONE', ( #6155, #6339, #8460 ) ) ;
#3671 = CARTESIAN_POINT ( 'NONE',  ( 25.29931031416560927, 192.8887977548965011, -27.79913727548661129 ) ) ;
#3672 = DIRECTION ( 'NONE',  ( -1.000000000000000000, -0.000000000000000000, -0.000000000000000000 ) ) ;
#3673 = EDGE_LOOP ( 'NONE', ( #488, #16999, #5436, #9273 ) ) ;
#3674 = ORIENTED_EDGE ( 'NONE', *, *, #15055, .T. ) ;
#3675 = ORIENTED_EDGE ( 'NONE', *, *, #4965, .F. ) ;
#3676 = VECTOR ( 'NONE', #6174, 1000.000000000000000 ) ;
#3677 = AXIS2_PLACEMENT_3D ( 'NONE', #13627, #16196, #10953 ) ;
#3678 = EDGE_CURVE ( 'NONE', #6832, #14506, #17348, .T. ) ;
#3679 = CARTESIAN_POINT ( 'NONE',  ( -86.80495063319472138, 149.8103701614163015, -24.76910924193870045 ) ) ;
#3680 = VECTOR ( 'NONE', #7873, 1000.000000000000000 ) ;
#3681 = ORIENTED_EDGE ( 'NONE', *, *, #2366, .F. ) ;
#3682 = CARTESIAN_POINT ( 'NONE',  ( -16.22141882056480355, 32.74469488918423821, 6.141726134091478606 ) ) ;
#3683 = CARTESIAN_POINT ( 'NONE',  ( 35.40819381912344710, 149.2475623141791061, -26.91697313366099920 ) ) ;
#3684 = PLANE ( 'NONE',  #760 ) ;
#3685 = CARTESIAN_POINT ( 'NONE',  ( 13.63270490666629975, 138.8028880870465969, 3.449993069226409581 ) ) ;
#3686 = ORIENTED_EDGE ( 'NONE', *, *, #10335, .F. ) ;
#3687 = CARTESIAN_POINT ( 'NONE',  ( 20.85969470496125666, 141.7883037112096929, 14.11015612222007398 ) ) ;
#3688 = CARTESIAN_POINT ( 'NONE',  ( 24.87028194210262910, 29.86925052300016858, -6.309743549972420595 ) ) ;
#3689 = DIRECTION ( 'NONE',  ( -1.000000000000000000, 0.000000000000000000, -8.673617379884037937E-17 ) ) ;
#3690 = DIRECTION ( 'NONE',  ( 1.000000000000000000, 0.000000000000000000, 0.000000000000000000 ) ) ;
#3691 = VECTOR ( 'NONE', #4231, 1000.000000000000000 ) ;
#3692 = CARTESIAN_POINT ( 'NONE',  ( -17.68452897573239824, 32.19524659542067013, -8.268362122121875046 ) ) ;
#3693 = ORIENTED_EDGE ( 'NONE', *, *, #16219, .F. ) ;
#3694 = DIRECTION ( 'NONE',  ( 0.000000000000000000, 0.000000000000000000, -1.000000000000000000 ) ) ;
#3695 = CARTESIAN_POINT ( 'NONE',  ( 28.44010998145314417, 201.3777828775944272, 14.27084532960636309 ) ) ;
#3696 = EDGE_LOOP ( 'NONE', ( #14809, #2667, #9669, #11653 ) ) ;
#3697 = ADVANCED_FACE ( 'NONE', ( #10615 ), #13545, .F. ) ;
#3698 = CYLINDRICAL_SURFACE ( 'NONE', #16338, 2.499999999999998668 ) ;
#3699 = DIRECTION ( 'NONE',  ( -2.674902700537819740E-31, 2.312964634635742267E-15, -1.000000000000000000 ) ) ;
#3700 = VECTOR ( 'NONE', #11958, 1000.000000000000000 ) ;
#3701 = ORIENTED_EDGE ( 'NONE', *, *, #16801, .T. ) ;
#3702 = CARTESIAN_POINT ( 'NONE',  ( -80.93218705276601099, 141.7051482704754335, 13.92628470286629749 ) ) ;
#3703 = FACE_OUTER_BOUND ( 'NONE', #6699, .T. ) ;
#3704 = CARTESIAN_POINT ( 'NONE',  ( -81.98700384596276081, 140.9569246592376714, -16.87109569490920435 ) ) ;
#3705 = EDGE_CURVE ( 'NONE', #2470, #13560, #518, .T. ) ;
#3706 = DIRECTION ( 'NONE',  ( 0.000000000000000000, 0.000000000000000000, 1.000000000000000000 ) ) ;
#3707 = EDGE_CURVE ( 'NONE', #7553, #399, #5892, .T. ) ;
#3708 = VERTEX_POINT ( 'NONE', #16209 ) ;
#3709 = PLANE ( 'NONE',  #10946 ) ;
#3710 = PLANE ( 'NONE',  #3949 ) ;
#3711 = APPLICATION_CONTEXT ( 'automotive_design' ) ;
#3712 = DIRECTION ( 'NONE',  ( 1.000000000000000000, -0.000000000000000000, -0.000000000000000000 ) ) ;
#3713 = CARTESIAN_POINT ( 'NONE',  ( 28.96355834781382654, 202.5339273643436400, -16.41656018636075487 ) ) ;
#3714 = ORIENTED_EDGE ( 'NONE', *, *, #12478, .T. ) ;
#3715 = CIRCLE ( 'NONE', #4287, 5.000000000000006217 ) ;
#3716 = ORIENTED_EDGE ( 'NONE', *, *, #1544, .T. ) ;
#3717 = ORIENTED_EDGE ( 'NONE', *, *, #14584, .T. ) ;
#3718 = CARTESIAN_POINT ( 'NONE',  ( 196.0000000000000000, 187.6227766016837961, 10.00000337241049309 ) ) ;
#3719 = ORIENTED_EDGE ( 'NONE', *, *, #10259, .T. ) ;
#3720 = CARTESIAN_POINT ( 'NONE',  ( -82.21997260166017440, 152.2013812635045156, -29.11730325185374113 ) ) ;
#3721 = CARTESIAN_POINT ( 'NONE',  ( 18.30724418481818461, 142.5286147297794344, -15.57621362570774437 ) ) ;
#3722 = ORIENTED_EDGE ( 'NONE', *, *, #17017, .F. ) ;
#3723 = DIRECTION ( 'NONE',  ( 0.000000000000000000, 0.000000000000000000, -1.000000000000000000 ) ) ;
#3724 = DIRECTION ( 'NONE',  ( -1.000000000000000000, -0.000000000000000000, -0.000000000000000000 ) ) ;
#3725 = VECTOR ( 'NONE', #11254, 1000.000000000000000 ) ;
#3726 = CARTESIAN_POINT ( 'NONE',  ( 48.00000000000000711, 175.6227766016838530, -19.42820660268601074 ) ) ;
#3727 = CARTESIAN_POINT ( 'NONE',  ( 30.00000000000000355, 196.6227766016838245, 10.00000000000000178 ) ) ;
#3728 = CARTESIAN_POINT ( 'NONE',  ( 24.00000000000000355, 146.6227766016838245, -35.00000000000000000 ) ) ;
#3729 = FACE_OUTER_BOUND ( 'NONE', #5733, .T. ) ;
#3730 = CARTESIAN_POINT ( 'NONE',  ( -23.66837786582113878, 18.00000000000000000, 17.32703391568840345 ) ) ;
#3731 = CARTESIAN_POINT ( 'NONE',  ( 30.00000000000000355, 196.6227766016838245, 0.000000000000000000 ) ) ;
#3732 = CARTESIAN_POINT ( 'NONE',  ( 48.00000000000000000, 171.6227766016838245, -10.00000337241048953 ) ) ;
#3733 = ORIENTED_EDGE ( 'NONE', *, *, #5759, .F. ) ;
#3734 = CARTESIAN_POINT ( 'NONE',  ( 48.00000000000000711, 191.6227766016837677, 8.071800142134975431 ) ) ;
#3735 = VERTEX_POINT ( 'NONE', #1421 ) ;
#3736 = DIRECTION ( 'NONE',  ( -1.000000000000000000, 0.000000000000000000, 0.000000000000000000 ) ) ;
#3737 = LINE ( 'NONE', #14526, #3292 ) ;
#3738 = EDGE_CURVE ( 'NONE', #12853, #7172, #10395, .T. ) ;
#3739 = ORIENTED_EDGE ( 'NONE', *, *, #11134, .F. ) ;
#3740 = CARTESIAN_POINT ( 'NONE',  ( -7.379000772444995526, 20.00000000000000000, 25.00000000000000000 ) ) ;
#3741 = CARTESIAN_POINT ( 'NONE',  ( 48.00000000000000711, 167.6227766016838814, 19.42820660268601074 ) ) ;
#3742 = LINE ( 'NONE', #14533, #15543 ) ;
#3743 = ORIENTED_EDGE ( 'NONE', *, *, #460, .T. ) ;
#3744 = CYLINDRICAL_SURFACE ( 'NONE', #14309, 2.500000000000000444 ) ;
#3745 = CARTESIAN_POINT ( 'NONE',  ( 25.11153254487453879, 190.9286879163519188, -26.76420670456568729 ) ) ;
#3746 = FACE_OUTER_BOUND ( 'NONE', #6834, .T. ) ;
#3747 = CARTESIAN_POINT ( 'NONE',  ( -12.63209758636618396, 17.99999999999999289, -7.167151760391626603 ) ) ;
#3748 = VERTEX_POINT ( 'NONE', #7778 ) ;
#3749 = DIRECTION ( 'NONE',  ( -1.000000000000000000, 0.000000000000000000, 0.000000000000000000 ) ) ;
#3750 = ORIENTED_EDGE ( 'NONE', *, *, #12229, .T. ) ;
#3751 = CARTESIAN_POINT ( 'NONE',  ( 35.54773459694453663, 194.3303362407250461, -26.63481108765544647 ) ) ;
#3752 = CARTESIAN_POINT ( 'NONE',  ( -38.00000000000000000, 20.00000000000000000, 30.00000000000000355 ) ) ;
#3753 = ADVANCED_FACE ( 'NONE', ( #5315 ), #10709, .T. ) ;
#3754 = VERTEX_POINT ( 'NONE', #15306 ) ;
#3755 = ADVANCED_FACE ( 'NONE', ( #5485 ), #15033, .T. ) ;
#3756 = EDGE_LOOP ( 'NONE', ( #14052, #411 ) ) ;
#3757 = EDGE_CURVE ( 'NONE', #5890, #4664, #5665, .T. ) ;
#3758 = VERTEX_POINT ( 'NONE', #11229 ) ;
#3759 = DIRECTION ( 'NONE',  ( -1.000000000000000000, -0.000000000000000000, 0.000000000000000000 ) ) ;
#3760 = ORIENTED_EDGE ( 'NONE', *, *, #13785, .F. ) ;
#3761 = DIRECTION ( 'NONE',  ( -1.000000000000000000, 0.000000000000000000, 0.000000000000000000 ) ) ;
#3762 = CARTESIAN_POINT ( 'NONE',  ( -24.93725393319378725, 100.0000000000000142, 5.500000000000000000 ) ) ;
#3763 = LINE ( 'NONE', #9153, #4505 ) ;
#3764 = CARTESIAN_POINT ( 'NONE',  ( 31.20232444244219394, 18.00000000000000000, 16.65183244245019623 ) ) ;
#3765 = CARTESIAN_POINT ( 'NONE',  ( -86.00000000000002842, 146.6227766016838245, -24.49489742783179480 ) ) ;
#3766 = ORIENTED_EDGE ( 'NONE', *, *, #9520, .F. ) ;
#3767 = FACE_OUTER_BOUND ( 'NONE', #9660, .T. ) ;
#3768 = CARTESIAN_POINT ( 'NONE',  ( -32.66708739526796279, 101.0000000000000142, -4.722170599040662609 ) ) ;
#3769 = CARTESIAN_POINT ( 'NONE',  ( 37.99999999999999289, 2.000000000000000000, 0.000000000000000000 ) ) ;
#3770 = CARTESIAN_POINT ( 'NONE',  ( 33.88556156013721932, 18.00000000000000000, 11.42442012027869858 ) ) ;
#3771 = CARTESIAN_POINT ( 'NONE',  ( -27.99999999999998224, 10.00000000000000000, 0.000000000000000000 ) ) ;
#3772 = VERTEX_POINT ( 'NONE', #4163 ) ;
#3773 = LINE ( 'NONE', #9259, #11466 ) ;
#3774 = CARTESIAN_POINT ( 'NONE',  ( 34.58999572048171700, 198.6265692133321465, 18.97388360722740686 ) ) ;
#3775 = EDGE_LOOP ( 'NONE', ( #3681, #9389 ) ) ;
#3776 = FILL_AREA_STYLE_COLOUR ( '', #15186 ) ;
#3777 = CARTESIAN_POINT ( 'NONE',  ( 34.99999999999999289, 8.000000000000000000, -35.00000000000002132 ) ) ;
#3778 = ORIENTED_EDGE ( 'NONE', *, *, #7387, .T. ) ;
#3779 = SURFACE_STYLE_FILL_AREA ( #14580 ) ;
#3780 = CARTESIAN_POINT ( 'NONE',  ( 34.93420767853316988, 30.00000000000000000, 0.000000000000000000 ) ) ;
#3781 = CARTESIAN_POINT ( 'NONE',  ( -85.49442651926489134, 144.1870492754457302, -21.73814637783849690 ) ) ;
#3782 = B_SPLINE_CURVE_WITH_KNOTS ( 'NONE', 3,
 ( #12505, #3296, #8333, #8521, #14012, #372, #10996, #13929, #1791, #16419, #13748, #16583, #14105, #4457, #7021, #4282, #12420, #9843, #12588, #4713, #14447, #3470 ),
 .UNSPECIFIED., .F., .F.,
 ( 4, 2, 2, 2, 2, 2, 2, 2, 2, 2, 4 ),
 ( 0.000000000000000000, 0.003698315653799323904, 0.007396631307598647807, 0.01109494696139797128, 0.01479326261519729561, 0.01664242044209697166, 0.01849157826899665291, 0.02218989392279601541, 0.02403905174969570360, 0.02588820957659539179, 0.02958652523039474735 ),
 .UNSPECIFIED. ) ;
#3783 = DIRECTION ( 'NONE',  ( -0.08715574274764661955, -0.4980973490458647235, -0.8627299156628267518 ) ) ;
#3784 = EDGE_LOOP ( 'NONE', ( #8150, #728, #10938 ) ) ;
#3785 = CARTESIAN_POINT ( 'NONE',  ( -45.00000000000000000, 130.0000000000000000, 15.00000000000000000 ) ) ;
#3786 = CARTESIAN_POINT ( 'NONE',  ( -207.5170152892447675, 173.3511749993040496, -4.985818809087040115 ) ) ;
#3787 = EDGE_CURVE ( 'NONE', #11737, #5404, #11814, .T. ) ;
#3788 = DIRECTION ( 'NONE',  ( -1.000000000000000000, -0.000000000000000000, 0.000000000000000000 ) ) ;
#3789 = UNCERTAINTY_MEASURE_WITH_UNIT (LENGTH_MEASURE( 1.000000000000000082E-05 ), #696, 'distance_accuracy_value', 'NONE');
#3790 = EDGE_CURVE ( 'NONE', #3368, #10746, #2205, .T. ) ;
#3791 = CARTESIAN_POINT ( 'NONE',  ( 35.49808778828385414, 199.0501964078081016, -21.74862058155258282 ) ) ;
#3792 = EDGE_LOOP ( 'NONE', ( #11666, #12149, #1078 ) ) ;
#3793 = VERTEX_POINT ( 'NONE', #1587 ) ;
#3794 = CARTESIAN_POINT ( 'NONE',  ( 7.559396570614633326, 133.9010074147453508, -14.92908841323498770 ) ) ;
#3795 = VECTOR ( 'NONE', #7709, 1000.000000000000000 ) ;
#3796 = VERTEX_POINT ( 'NONE', #16648 ) ;
#3797 = CARTESIAN_POINT ( 'NONE',  ( -86.00000000000001421, 146.9394831494155937, -24.81813469455733667 ) ) ;
#3798 = EDGE_CURVE ( 'NONE', #8505, #1185, #8301, .T. ) ;
#3799 = CARTESIAN_POINT ( 'NONE',  ( 8.997728150919979129, 132.8900016178789372, -12.55705910147062099 ) ) ;
#3800 = EDGE_CURVE ( 'NONE', #17452, #7206, #7303, .T. ) ;
#3801 = ORIENTED_EDGE ( 'NONE', *, *, #12863, .F. ) ;
#3802 = CARTESIAN_POINT ( 'NONE',  ( 196.0000000000000000, 183.6227766016837961, -5.571800142134975431 ) ) ;
#3803 = DIRECTION ( 'NONE',  ( 1.000000000000000000, 0.000000000000000000, 0.000000000000000000 ) ) ;
#3804 = CARTESIAN_POINT ( 'NONE',  ( 24.72505082391212028, 201.9542783778900059, -13.00000000000000000 ) ) ;
#3805 = LINE ( 'NONE', #1237, #3298 ) ;
#3806 = DIRECTION ( 'NONE',  ( -1.000000000000000000, 0.000000000000000000, 0.000000000000000000 ) ) ;
#3807 = AXIS2_PLACEMENT_3D ( 'NONE', #10623, #3912, #10267 ) ;
#3808 = AXIS2_PLACEMENT_3D ( 'NONE', #8012, #6427, #17224 ) ;
#3809 = CARTESIAN_POINT ( 'NONE',  ( 23.09107716925733911, 18.00000000000000355, -5.000000000000003553 ) ) ;
#3810 = CARTESIAN_POINT ( 'NONE',  ( 1.559999999999998943, -1.732050807568885631, 0.000000000000000000 ) ) ;
#3811 = CARTESIAN_POINT ( 'NONE',  ( -80.00000000000002842, 146.6227766016838245, -35.00200000000000244 ) ) ;
#3812 = AXIS2_PLACEMENT_3D ( 'NONE', #16580, #16674, #291 ) ;
#3813 = CARTESIAN_POINT ( 'NONE',  ( -103.0000000000000142, 171.6227766016838245, 0.000000000000000000 ) ) ;
#3814 = EDGE_CURVE ( 'NONE', #14287, #5825, #4484, .T. ) ;
#3815 = CARTESIAN_POINT ( 'NONE',  ( 24.16536605930837212, 145.1786002333612089, -22.93437194230014242 ) ) ;
#3816 = EDGE_LOOP ( 'NONE', ( #16162, #7840, #326, #3008 ) ) ;
#3817 = CARTESIAN_POINT ( 'NONE',  ( -82.50000000000002842, 146.6227766016838245, 10.00000000000000178 ) ) ;
#3818 = ORIENTED_EDGE ( 'NONE', *, *, #8673, .F. ) ;
#3819 = DIRECTION ( 'NONE',  ( 0.000000000000000000, 0.000000000000000000, -1.000000000000000000 ) ) ;
#3820 = EDGE_CURVE ( 'NONE', #6443, #10551, #16911, .T. ) ;
#3821 = CARTESIAN_POINT ( 'NONE',  ( -20.85266279178582138, 18.00000000000000000, -20.15433268689461954 ) ) ;
#3822 = ORIENTED_EDGE ( 'NONE', *, *, #1619, .F. ) ;
#3823 = EDGE_CURVE ( 'NONE', #9326, #730, #1649, .T. ) ;
#3824 = CARTESIAN_POINT ( 'NONE',  ( -68.00000000000000000, 171.6227766016838245, -20.00000000000000355 ) ) ;
#3825 = EDGE_CURVE ( 'NONE', #3708, #9609, #6987, .T. ) ;
#3826 = CARTESIAN_POINT ( 'NONE',  ( 14.24850047812951104, 138.6393229685333779, 3.919138222309279218 ) ) ;
#3827 = AXIS2_PLACEMENT_3D ( 'NONE', #10507, #5024, #10415 ) ;
#3828 = ORIENTED_EDGE ( 'NONE', *, *, #9046, .F. ) ;
#3829 = STYLED_ITEM ( 'NONE', ( #7859 ), #11216 ) ;
#3830 = CARTESIAN_POINT ( 'NONE',  ( 17.53546816055562374, 19.99999999999999645, 24.87355917367628422 ) ) ;
#3831 = CIRCLE ( 'NONE', #2124, 8.000000000000000000 ) ;
#3832 = AXIS2_PLACEMENT_3D ( 'NONE', #5185, #15987, #16179 ) ;
#3833 = EDGE_LOOP ( 'NONE', ( #9654, #1189, #9148, #16548, #14428, #10658, #5494 ) ) ;
#3834 = CYLINDRICAL_SURFACE ( 'NONE', #12341, 5.000000000000006217 ) ;
#3835 = CARTESIAN_POINT ( 'NONE',  ( 22.50000000000000711, 196.2479045481293269, -21.97573418327509742 ) ) ;
#3836 = FACE_OUTER_BOUND ( 'NONE', #3580, .T. ) ;
#3837 = ADVANCED_FACE ( 'NONE', ( #11056 ), #8398, .F. ) ;
#3838 = CARTESIAN_POINT ( 'NONE',  ( -11.31385407355777950, 31.26810920821015216, -12.21116371260378308 ) ) ;
#3839 = MECHANICAL_DESIGN_GEOMETRIC_PRESENTATION_REPRESENTATION (  '', ( #1297 ), #13733 ) ;
#3840 = VERTEX_POINT ( 'NONE', #1847 ) ;
#3841 = CARTESIAN_POINT ( 'NONE',  ( 0.000000000000000000, 0.000000000000000000, 0.000000000000000000 ) ) ;
#3842 = VECTOR ( 'NONE', #6700, 1000.000000000000000 ) ;
#3843 = ORIENTED_EDGE ( 'NONE', *, *, #11224, .T. ) ;
#3844 = CARTESIAN_POINT ( 'NONE',  ( 24.10475933960641370, 195.4942584061381865, -25.59693137756977421 ) ) ;
#3845 = CARTESIAN_POINT ( 'NONE',  ( 49.99999999999998579, 183.6227766016837961, 8.071800142134975431 ) ) ;
#3846 = B_SPLINE_CURVE_WITH_KNOTS ( 'NONE', 3,
 ( #9511, #1647, #13776, #8275, #5718, #11107, #16518, #4390, #7130, #12529, #395, #11190, #1813, #14922, #5796, #2800, #16609, #483, #10845, #8193, #1476, #12264, #137, #10928, #16351 ),
 .UNSPECIFIED., .F., .F.,
 ( 4, 2, 2, 1, 2, 2, 2, 2, 2, 2, 2, 2, 4 ),
 ( 0.000000000000000000, 0.003937549356687076833, 0.005906324035030613949, 0.007875098713374151932, 0.009843873391717689048, 0.01181264807006122616, 0.01575019742674830733, 0.01771897210509184445, 0.01968774678343538503, 0.02362529614012245927, 0.02559407081846599985, 0.02756284549680953697, 0.03150039485349661467 ),
 .UNSPECIFIED. ) ;
#3847 = VECTOR ( 'NONE', #6109, 1000.000000000000000 ) ;
#3848 = ORIENTED_EDGE ( 'NONE', *, *, #13272, .T. ) ;
#3849 = ORIENTED_EDGE ( 'NONE', *, *, #2108, .F. ) ;
#3850 = ORIENTED_EDGE ( 'NONE', *, *, #16742, .F. ) ;
#3851 = DIRECTION ( 'NONE',  ( -2.507721281754210796E-32, -1.000000000000000000, 2.891205793294676354E-16 ) ) ;
#3852 = UNCERTAINTY_MEASURE_WITH_UNIT (LENGTH_MEASURE( 1.000000000000000082E-05 ), #3163, 'distance_accuracy_value', 'NONE');
#3853 = CIRCLE ( 'NONE', #13744, 2.500000000000000444 ) ;
#3854 = CIRCLE ( 'NONE', #12326, 30.00000000000000000 ) ;
#3855 = EDGE_LOOP ( 'NONE', ( #3153, #2014, #10255, #1909 ) ) ;
#3856 = CARTESIAN_POINT ( 'NONE',  ( -9.527527117355448993, 30.70225384978374450, 12.78416694138776855 ) ) ;
#3857 = VECTOR ( 'NONE', #3672, 1000.000000000000000 ) ;
#3858 = CARTESIAN_POINT ( 'NONE',  ( -17.03105419742079363, 32.06459626301238330, 9.633022903854756791 ) ) ;
#3859 = CARTESIAN_POINT ( 'NONE',  ( 25.17791007590961172, 150.1982800653300387, -27.67726561134454144 ) ) ;
#3860 = ADVANCED_FACE ( 'NONE', ( #16470 ), #12215, .F. ) ;
#3861 = CARTESIAN_POINT ( 'NONE',  ( 20.28823715622366919, 18.00000000000000000, 11.10707270023369730 ) ) ;
#3862 = EDGE_CURVE ( 'NONE', #374, #8817, #16644, .T. ) ;
#3863 = CARTESIAN_POINT ( 'NONE',  ( -78.11096775391246183, 151.2561509761041805, 25.96550485207006886 ) ) ;
#3864 = EDGE_CURVE ( 'NONE', #1301, #9238, #2786, .T. ) ;
#3865 = ORIENTED_EDGE ( 'NONE', *, *, #2879, .F. ) ;
#3866 = CARTESIAN_POINT ( 'NONE',  ( 24.26130280265436667, 140.5733633045254578, 11.19213049117091785 ) ) ;
#3867 = CARTESIAN_POINT ( 'NONE',  ( 34.93420767853316988, 20.00000000000000000, 15.00000000000000000 ) ) ;
#3868 = CARTESIAN_POINT ( 'NONE',  ( -22.99999999999999289, 90.00000000000000000, 15.00000000000000000 ) ) ;
#3869 = CARTESIAN_POINT ( 'NONE',  ( -100.0000000000000000, 120.0000000000000284, -6.000000000000001776 ) ) ;
#3870 = CARTESIAN_POINT ( 'NONE',  ( 24.41053355130577884, 29.87514852601161763, 8.212591972297857978 ) ) ;
#3871 = VERTEX_POINT ( 'NONE', #12477 ) ;
#3872 = CARTESIAN_POINT ( 'NONE',  ( 15.00000000000000000, 191.6227766016837961, -1.224646799147353454E-15 ) ) ;
#3873 = AXIS2_PLACEMENT_3D ( 'NONE', #14623, #4015, #17187 ) ;
#3874 = VECTOR ( 'NONE', #3464, 1000.000000000000000 ) ;
#3875 = VECTOR ( 'NONE', #11057, 1000.000000000000114 ) ;
#3876 = CARTESIAN_POINT ( 'NONE',  ( 29.85838552320831951, 201.6221756766237831, 13.74903839801206296 ) ) ;
#3877 = EDGE_LOOP ( 'NONE', ( #4904, #2393 ) ) ;
#3878 = CARTESIAN_POINT ( 'NONE',  ( -40.00000000000000000, 20.00000000000000000, -28.00000000000000355 ) ) ;
#3879 = DIRECTION ( 'NONE',  ( 0.000000000000000000, 0.000000000000000000, 1.000000000000000000 ) ) ;
#3880 = ORIENTED_EDGE ( 'NONE', *, *, #16098, .T. ) ;
#3881 = CARTESIAN_POINT ( 'NONE',  ( -79.76724320816964564, 141.6224873770942736, 13.74709594552941105 ) ) ;
#3882 = CARTESIAN_POINT ( 'NONE',  ( 48.00000000000000711, 167.6227766016838530, 3.071800142134975431 ) ) ;
#3883 = CARTESIAN_POINT ( 'NONE',  ( -100.0000000000000000, 143.0439382767972347, -16.49999999999984368 ) ) ;
#3884 = EDGE_CURVE ( 'NONE', #13912, #15454, #12673, .T. ) ;
#3885 = AXIS2_PLACEMENT_3D ( 'NONE', #14870, #7084, #10803 ) ;
#3886 = CARTESIAN_POINT ( 'NONE',  ( -187.6513770290094669, 169.2829632032627103, 0.3407269638998700612 ) ) ;
#3887 =( GEOMETRIC_REPRESENTATION_CONTEXT ( 3 ) GLOBAL_UNCERTAINTY_ASSIGNED_CONTEXT ( ( #17305 ) ) GLOBAL_UNIT_ASSIGNED_CONTEXT ( ( #11826, #10317, #1034 ) ) REPRESENTATION_CONTEXT ( 'NONE', 'WORKASPACE' ) );
#3888 = EDGE_LOOP ( 'NONE', ( #13542, #6426, #2824, #14641 ) ) ;
#3889 = DIRECTION ( 'NONE',  ( 1.000000000000000000, -0.000000000000000000, -0.000000000000000000 ) ) ;
#3890 = DIRECTION ( 'NONE',  ( 2.312964634635742464E-16, 0.000000000000000000, -1.000000000000000000 ) ) ;
#3891 = CARTESIAN_POINT ( 'NONE',  ( 35.49999999999998579, 9.999999999999998224, -35.00200000000000244 ) ) ;
#3892 = LINE ( 'NONE', #12119, #10030 ) ;
#3893 = ORIENTED_EDGE ( 'NONE', *, *, #3030, .F. ) ;
#3894 = CARTESIAN_POINT ( 'NONE',  ( -45.00000000000000711, 171.6227766016838245, 5.000000000000007994 ) ) ;
#3895 = AXIS2_PLACEMENT_3D ( 'NONE', #1138, #3889, #14500 ) ;
#3896 = ORIENTED_EDGE ( 'NONE', *, *, #15638, .T. ) ;
#3897 = PRODUCT_DEFINITION_FORMATION_WITH_SPECIFIED_SOURCE ( 'ANY', '', #15498, .NOT_KNOWN. ) ;
#3898 = FACE_BOUND ( 'NONE', #16396, .T. ) ;
#3899 = AXIS2_PLACEMENT_3D ( 'NONE', #14295, #3851, #851 ) ;
#3900 = CARTESIAN_POINT ( 'NONE',  ( 13.35668486245713282, 128.6964509245273405, -9.918424562684259982 ) ) ;
#3901 = ORIENTED_EDGE ( 'NONE', *, *, #12113, .F. ) ;
#3902 = CYLINDRICAL_SURFACE ( 'NONE', #4468, 20.00000000000000355 ) ;
#3903 = CARTESIAN_POINT ( 'NONE',  ( 25.49999999999998579, 9.999999999999998224, -16.00000000000000000 ) ) ;
#3904 = ADVANCED_FACE ( 'NONE', ( #8491 ), #13815, .T. ) ;
#3905 = CARTESIAN_POINT ( 'NONE',  ( 22.56345771982927317, 197.7288430733995312, -20.20458554073936241 ) ) ;
#3906 = DIRECTION ( 'NONE',  ( 0.000000000000000000, 1.000000000000000000, 0.000000000000000000 ) ) ;
#3907 = DIRECTION ( 'NONE',  ( 0.000000000000000000, 0.000000000000000000, 1.000000000000000000 ) ) ;
#3908 = CARTESIAN_POINT ( 'NONE',  ( 17.75267852353177034, 29.94338869414745830, -12.49131726690029254 ) ) ;
#3909 = DIRECTION ( 'NONE',  ( -1.000000000000000000, 0.000000000000000000, 1.541976423090495387E-16 ) ) ;
#3910 = CARTESIAN_POINT ( 'NONE',  ( -100.0000000000000000, 141.6227766016838245, 0.000000000000000000 ) ) ;
#3911 = VECTOR ( 'NONE', #12611, 1000.000000000000000 ) ;
#3912 = DIRECTION ( 'NONE',  ( -0.000000000000000000, -0.000000000000000000, 1.000000000000000000 ) ) ;
#3913 =( GEOMETRIC_REPRESENTATION_CONTEXT ( 3 ) GLOBAL_UNCERTAINTY_ASSIGNED_CONTEXT ( ( #4233 ) ) GLOBAL_UNIT_ASSIGNED_CONTEXT ( ( #5828, #12646, #4678 ) ) REPRESENTATION_CONTEXT ( 'NONE', 'WORKASPACE' ) );
#3914 =( NAMED_UNIT ( * ) SI_UNIT ( $, .STERADIAN. ) SOLID_ANGLE_UNIT ( ) );
#3915 = ORIENTED_EDGE ( 'NONE', *, *, #623, .T. ) ;
#3916 = CARTESIAN_POINT ( 'NONE',  ( 11.07991637643875116, 132.1496266960828336, -13.91448104906911709 ) ) ;
#3917 = ORIENTED_EDGE ( 'NONE', *, *, #16200, .T. ) ;
#3918 = CARTESIAN_POINT ( 'NONE',  ( -80.00000000000001421, 196.6227766016838245, 1.387778780781445676E-14 ) ) ;
#3919 = DIRECTION ( 'NONE',  ( 0.000000000000000000, 0.000000000000000000, -1.000000000000000000 ) ) ;
#3920 = ADVANCED_FACE ( 'NONE', ( #12558 ), #12650, .F. ) ;
#3921 = ORIENTED_EDGE ( 'NONE', *, *, #458, .F. ) ;
#3922 = CARTESIAN_POINT ( 'NONE',  ( -8.792264229871568304, 30.31966024794114745, 14.93731107458715357 ) ) ;
#3923 = CARTESIAN_POINT ( 'NONE',  ( 12.74723713713078155, 129.4272226793184473, 10.49625762048852451 ) ) ;
#3924 = ORIENTED_EDGE ( 'NONE', *, *, #7277, .F. ) ;
#3925 = AXIS2_PLACEMENT_3D ( 'NONE', #6291, #977, #2394 ) ;
#3926 = CARTESIAN_POINT ( 'NONE',  ( 19.47274266584531333, 19.99999999999999645, 24.48069943974461538 ) ) ;
#3927 = EDGE_CURVE ( 'NONE', #9465, #10480, #11324, .T. ) ;
#3928 = AXIS2_PLACEMENT_3D ( 'NONE', #13888, #16532, #330 ) ;
#3929 = VERTEX_POINT ( 'NONE', #2193 ) ;
#3930 = EDGE_CURVE ( 'NONE', #9467, #4581, #11658, .T. ) ;
#3931 = DIRECTION ( 'NONE',  ( 1.000000000000000000, 0.000000000000000000, 0.000000000000000000 ) ) ;
#3932 = FACE_OUTER_BOUND ( 'NONE', #9451, .T. ) ;
#3933 = CARTESIAN_POINT ( 'NONE',  ( -73.00000000000001421, 171.6227766016838245, -19.49999999999998934 ) ) ;
#3934 = CARTESIAN_POINT ( 'NONE',  ( -15.37626115774789248, 32.49812920269235406, -8.581855491731886332 ) ) ;
#3935 = EDGE_CURVE ( 'NONE', #11848, #12781, #13002, .T. ) ;
#3936 = EDGE_CURVE ( 'NONE', #11405, #7894, #9852, .T. ) ;
#3937 = ORIENTED_EDGE ( 'NONE', *, *, #10878, .F. ) ;
#3938 = CARTESIAN_POINT ( 'NONE',  ( 25.00000000000000711, 146.6227766016838245, 21.54065922853802562 ) ) ;
#3939 = AXIS2_PLACEMENT_3D ( 'NONE', #15039, #1770, #2834 ) ;
#3940 = AXIS2_PLACEMENT_3D ( 'NONE', #16610, #11375, #10129 ) ;
#3941 = ORIENTED_EDGE ( 'NONE', *, *, #10282, .F. ) ;
#3942 = CARTESIAN_POINT ( 'NONE',  ( -87.47214505283551489, 195.8611292878214272, -22.40167687543583952 ) ) ;
#3943 = AXIS2_PLACEMENT_3D ( 'NONE', #17491, #11017, #576 ) ;
#3944 = CARTESIAN_POINT ( 'NONE',  ( -3.000000000000002665, 134.2062027339443944, 25.00000000000000000 ) ) ;
#3945 = ORIENTED_EDGE ( 'NONE', *, *, #9705, .F. ) ;
#3946 = VERTEX_POINT ( 'NONE', #4680 ) ;
#3947 = VERTEX_POINT ( 'NONE', #6267 ) ;
#3948 = DIRECTION ( 'NONE',  ( 1.000000000000000000, 0.000000000000000000, 0.000000000000000000 ) ) ;
#3949 = AXIS2_PLACEMENT_3D ( 'NONE', #14501, #17335, #9441 ) ;
#3950 = EDGE_LOOP ( 'NONE', ( #9098, #10342, #13186, #12335 ) ) ;
#3951 = CARTESIAN_POINT ( 'NONE',  ( 0.000000000000000000, 0.000000000000000000, 0.000000000000000000 ) ) ;
#3952 = CIRCLE ( 'NONE', #4794, 9.999999999999998224 ) ;
#3953 = CARTESIAN_POINT ( 'NONE',  ( -7.922882945419460476, 30.18055256556250399, 13.00000000000000355 ) ) ;
#3954 = AXIS2_PLACEMENT_3D ( 'NONE', #11673, #2121, #17006 ) ;
#3955 = CARTESIAN_POINT ( 'NONE',  ( -15.37994105483213758, 31.72997864396344525, 11.82123051499886479 ) ) ;
#3956 = DIRECTION ( 'NONE',  ( 2.312964634635742464E-16, 0.000000000000000000, 1.000000000000000000 ) ) ;
#3957 = DIRECTION ( 'NONE',  ( 1.000000000000000000, 0.000000000000000000, 0.000000000000000000 ) ) ;
#3958 = CARTESIAN_POINT ( 'NONE',  ( -80.20949202752900931, 151.6222428389255015, 26.24840280143448368 ) ) ;
#3959 = ORIENTED_EDGE ( 'NONE', *, *, #7710, .F. ) ;
#3960 = FACE_BOUND ( 'NONE', #4868, .T. ) ;
#3961 = CARTESIAN_POINT ( 'NONE',  ( 19.94005785806629660, 29.93324777864367192, -13.66280195656096907 ) ) ;
#3962 = DIRECTION ( 'NONE',  ( -1.000000000000000000, -0.000000000000000000, -0.000000000000000000 ) ) ;
#3963 = CARTESIAN_POINT ( 'NONE',  ( 23.79315516583586643, 18.00000000000000000, 22.94240041036162836 ) ) ;
#3964 = DIRECTION ( 'NONE',  ( 1.000000000000000000, 0.000000000000000000, 0.000000000000000000 ) ) ;
#3965 = ORIENTED_EDGE ( 'NONE', *, *, #17384, .F. ) ;
#3966 = CARTESIAN_POINT ( 'NONE',  ( -85.59761955342212048, 141.6105225557631115, -13.74486639216964612 ) ) ;
#3967 = AXIS2_PLACEMENT_3D ( 'NONE', #8293, #14939, #8031 ) ;
#3968 = CIRCLE ( 'NONE', #6217, 4.750000000000000000 ) ;
#3969 = CARTESIAN_POINT ( 'NONE',  ( 49.99999999999998579, 175.6227766016838530, -19.42820660268601074 ) ) ;
#3970 = DIRECTION ( 'NONE',  ( -1.000000000000000000, -0.000000000000000000, -0.000000000000000000 ) ) ;
#3971 = EDGE_CURVE ( 'NONE', #12127, #1460, #5551, .T. ) ;
#3972 = VERTEX_POINT ( 'NONE', #14322 ) ;
#3973 = CARTESIAN_POINT ( 'NONE',  ( -32.43085388486576193, 100.3453498474263910, -5.312352690998809912 ) ) ;
#3974 = ORIENTED_EDGE ( 'NONE', *, *, #8981, .T. ) ;
#3975 = EDGE_CURVE ( 'NONE', #14680, #16221, #10130, .T. ) ;
#3976 = DIRECTION ( 'NONE',  ( -0.000000000000000000, -0.000000000000000000, -1.000000000000000000 ) ) ;
#3977 = CARTESIAN_POINT ( 'NONE',  ( 16.62686111071178630, 17.99999999999942801, -12.85442640772723344 ) ) ;
#3978 = AXIS2_PLACEMENT_3D ( 'NONE', #8826, #8563, #16727 ) ;
#3979 = CARTESIAN_POINT ( 'NONE',  ( -84.06337902274010787, 142.1921853732337979, -18.94830881272694256 ) ) ;
#3980 = CIRCLE ( 'NONE', #11317, 2.499999999999998668 ) ;
#3981 = VECTOR ( 'NONE', #1011, 1000.000000000000000 ) ;
#3982 = CARTESIAN_POINT ( 'NONE',  ( -22.79696676584442017, 19.99999999999999645, 18.34105320469109301 ) ) ;
#3983 = ORIENTED_EDGE ( 'NONE', *, *, #17160, .F. ) ;
#3984 = DIRECTION ( 'NONE',  ( 1.000000000000000000, 0.000000000000000000, 0.000000000000000000 ) ) ;
#3985 = LINE ( 'NONE', #2644, #4236 ) ;
#3986 = DIRECTION ( 'NONE',  ( -1.000000000000000000, 0.000000000000000000, 0.000000000000000000 ) ) ;
#3987 = CARTESIAN_POINT ( 'NONE',  ( -5.000000000000000888, 191.6227766016837961, -1.224646799147353454E-15 ) ) ;
#3988 = EDGE_LOOP ( 'NONE', ( #1715, #11625, #16732, #16116 ) ) ;
#3989 = AXIS2_PLACEMENT_3D ( 'NONE', #5717, #3227, #11105 ) ;
#3990 = CARTESIAN_POINT ( 'NONE',  ( 9.647168043681871197, 132.9898913927504225, -14.44632387683999575 ) ) ;
#3991 = EDGE_CURVE ( 'NONE', #5446, #14731, #14114, .T. ) ;
#3992 = EDGE_CURVE ( 'NONE', #453, #14270, #12822, .T. ) ;
#3993 = EDGE_CURVE ( 'NONE', #9130, #2572, #15479, .T. ) ;
#3994 = EDGE_LOOP ( 'NONE', ( #6545, #7729, #7726, #11711 ) ) ;
#3995 = DIRECTION ( 'NONE',  ( 0.000000000000000000, 0.000000000000000000, 1.000000000000000000 ) ) ;
#3996 = CIRCLE ( 'NONE', #4556, 5.000000000000000888 ) ;
#3997 = CARTESIAN_POINT ( 'NONE',  ( 23.14977753070779087, 141.0007991078602743, -12.30735618844933832 ) ) ;
#3998 = ORIENTED_EDGE ( 'NONE', *, *, #10405, .T. ) ;
#3999 = DIRECTION ( 'NONE',  ( -1.000000000000000000, -0.000000000000000000, -0.000000000000000000 ) ) ;
#4000 = CARTESIAN_POINT ( 'NONE',  ( -3.000000000000000888, 154.3022685259950038, 9.999999999999900524 ) ) ;
#4001 = PLANE ( 'NONE',  #3626 ) ;
#4002 = DIRECTION ( 'NONE',  ( -1.000000000000000000, -0.000000000000000000, -0.000000000000000000 ) ) ;
#4003 = CARTESIAN_POINT ( 'NONE',  ( 49.99999999999998579, 151.6227766016839098, -5.571800142134973655 ) ) ;
#4004 = CARTESIAN_POINT ( 'NONE',  ( 21.99569976772868074, 17.99999999999999645, -9.076888812463767664 ) ) ;
#4005 = CARTESIAN_POINT ( 'NONE',  ( -197.9999999999999716, 171.6227766016838245, 0.000000000000000000 ) ) ;
#4006 = AXIS2_PLACEMENT_3D ( 'NONE', #12522, #386, #16602 ) ;
#4007 = DIRECTION ( 'NONE',  ( -1.000000000000000000, 0.000000000000000000, 0.000000000000000000 ) ) ;
#4008 = CYLINDRICAL_SURFACE ( 'NONE', #13003, 2.500000000000000444 ) ;
#4009 = DIRECTION ( 'NONE',  ( 1.000000000000000000, 0.000000000000000000, 0.000000000000000000 ) ) ;
#4010 = ORIENTED_EDGE ( 'NONE', *, *, #1057, .T. ) ;
#4011 = CARTESIAN_POINT ( 'NONE',  ( 16.69631138515844171, 126.9345490261019904, -8.565329098038530375 ) ) ;
#4012 = ORIENTED_EDGE ( 'NONE', *, *, #6850, .F. ) ;
#4013 = EDGE_CURVE ( 'NONE', #10750, #5523, #14167, .T. ) ;
#4014 = CARTESIAN_POINT ( 'NONE',  ( 27.99999999999998224, 9.999999999999998224, 10.00000000000000178 ) ) ;
#4015 = DIRECTION ( 'NONE',  ( -1.000000000000000000, 0.000000000000000000, 0.000000000000000000 ) ) ;
#4016 = ORIENTED_EDGE ( 'NONE', *, *, #8405, .F. ) ;
#4017 = CARTESIAN_POINT ( 'NONE',  ( -16.41264213764281976, 19.99999999999999645, 23.02790928165778794 ) ) ;
#4018 = CARTESIAN_POINT ( 'NONE',  ( 14.40670567839409344, 127.3124839991112083, 8.619616438334361419 ) ) ;
#4019 = ORIENTED_EDGE ( 'NONE', *, *, #661, .T. ) ;
#4020 = CYLINDRICAL_SURFACE ( 'NONE', #10166, 5.000000000000007994 ) ;
#4021 = ORIENTED_EDGE ( 'NONE', *, *, #11179, .T. ) ;
#4022 = DIRECTION ( 'NONE',  ( 0.000000000000000000, -0.8660254037844413721, 0.4999999999999953371 ) ) ;
#4023 = CARTESIAN_POINT ( 'NONE',  ( -207.8780901672883488, 175.5271247293819386, 3.924367008119225453 ) ) ;
#4024 = DIRECTION ( 'NONE',  ( -1.000000000000000000, -0.000000000000000000, 0.000000000000000000 ) ) ;
#4025 = DIRECTION ( 'NONE',  ( 0.000000000000000000, 0.000000000000000000, -1.000000000000000000 ) ) ;
#4026 = B_SPLINE_CURVE_WITH_KNOTS ( 'NONE', 3,
 ( #4979, #3835, #11790, #1177, #9315, #17195, #5070, #3567, #15875, #10548, #10470, #11694, #6488, #14538, #3745, #7806, #10371, #10646, #17107, #9132, #9225, #15782, #15956, #14634, #7902, #6581, #5243, #16055, #7549, #8962, #14373, #13483, #9484, #13393, #15056, #6917, #16231, #4189, #5341, #11077, #1615, #7015, #6762, #1357, #2683, #8071 ),
 .UNSPECIFIED., .F., .F.,
 ( 4, 2, 2, 2, 2, 2, 2, 2, 2, 2, 2, 2, 2, 2, 2, 2, 2, 2, 2, 2, 2, 2, 4 ),
 ( 0.01035378412632265502, 0.01206629175607490910, 0.01377879938582716318, 0.01549130701557941726, 0.01634756083045556946, 0.01720381464533172339, 0.01806006846020787732, 0.01891632227508402778, 0.02062882990483638768, 0.02148508371971258324, 0.02234133753458877880, 0.02319759134946497436, 0.02405384516434117687, 0.02576635279409356799, 0.02747886042384597299, 0.02833511423872216509, 0.02919136805359836065, 0.03090387568335074484, 0.03261638331310313943, 0.03432889094285552362, 0.03604139857260790780, 0.03689765238748410336, 0.03775390620236029199 ),
 .UNSPECIFIED. ) ;
#4027 = ORIENTED_EDGE ( 'NONE', *, *, #5596, .F. ) ;
#4028 = CARTESIAN_POINT ( 'NONE',  ( 29.20274480926571314, 151.5627461462769929, 26.20297826401937158 ) ) ;
#4029 = EDGE_CURVE ( 'NONE', #4990, #13903, #10247, .T. ) ;
#4030 = ORIENTED_EDGE ( 'NONE', *, *, #3638, .F. ) ;
#4031 = ADVANCED_FACE ( 'NONE', ( #6092 ), #3263, .F. ) ;
#4032 = FACE_OUTER_BOUND ( 'NONE', #3784, .T. ) ;
#4033 = LINE ( 'NONE', #10379, #3857 ) ;
#4034 = ORIENTED_EDGE ( 'NONE', *, *, #3483, .F. ) ;
#4035 = ORIENTED_EDGE ( 'NONE', *, *, #15780, .T. ) ;
#4036 = ORIENTED_EDGE ( 'NONE', *, *, #14985, .F. ) ;
#4037 = CARTESIAN_POINT ( 'NONE',  ( 12.89436750745977278, 141.9634372303913779, 18.58317047499899743 ) ) ;
#4038 = EDGE_CURVE ( 'NONE', #1489, #8410, #14077, .T. ) ;
#4039 = ADVANCED_FACE ( 'NONE', ( #1938 ), #7339, .F. ) ;
#4040 = ORIENTED_EDGE ( 'NONE', *, *, #13391, .T. ) ;
#4041 = CARTESIAN_POINT ( 'NONE',  ( -116.4755503550297107, 171.6227766016838245, 78.75916623668499028 ) ) ;
#4042 = CARTESIAN_POINT ( 'NONE',  ( 30.00000000000000355, 196.6227766016838245, -16.00000000000000000 ) ) ;
#4043 = CYLINDRICAL_SURFACE ( 'NONE', #11282, 5.000000000000000888 ) ;
#4044 = DIRECTION ( 'NONE',  ( 1.000000000000000000, -0.000000000000000000, -0.000000000000000000 ) ) ;
#4045 = CARTESIAN_POINT ( 'NONE',  ( -76.34554854693054438, 150.0509117818997709, 24.97535314687243613 ) ) ;
#4046 = VERTEX_POINT ( 'NONE', #10163 ) ;
#4047 = CARTESIAN_POINT ( 'NONE',  ( 30.00000000000000355, 196.6227766016838245, 0.000000000000000000 ) ) ;
#4048 = DIRECTION ( 'NONE',  ( -1.000000000000000000, -0.000000000000000000, -0.000000000000000000 ) ) ;
#4049 = CARTESIAN_POINT ( 'NONE',  ( 13.34250444320487361, 130.4016344817123070, 12.56142338728217744 ) ) ;
#4050 = CARTESIAN_POINT ( 'NONE',  ( 28.15871609335591685, 18.00000000000000000, 20.05978710182010971 ) ) ;
#4051 = DIRECTION ( 'NONE',  ( -0.000000000000000000, -0.000000000000000000, -1.000000000000000000 ) ) ;
#4052 = DIRECTION ( 'NONE',  ( 0.000000000000000000, 0.000000000000000000, 1.000000000000000000 ) ) ;
#4053 = FACE_OUTER_BOUND ( 'NONE', #7266, .T. ) ;
#4054 = VERTEX_POINT ( 'NONE', #15646 ) ;
#4055 = DIRECTION ( 'NONE',  ( 0.000000000000000000, -1.000000000000000000, 0.000000000000000000 ) ) ;
#4056 = EDGE_CURVE ( 'NONE', #8410, #5512, #9279, .T. ) ;
#4057 = ORIENTED_EDGE ( 'NONE', *, *, #658, .T. ) ;
#4058 = DIRECTION ( 'NONE',  ( 1.000000000000000000, 0.000000000000000000, 0.000000000000000000 ) ) ;
#4059 = CARTESIAN_POINT ( 'NONE',  ( 17.00000000000000000, 154.3022685259950038, -9.999999999999900524 ) ) ;
#4060 = CARTESIAN_POINT ( 'NONE',  ( -85.83463394069167407, 145.1786002333612089, -22.93437194230014242 ) ) ;
#4061 = CYLINDRICAL_SURFACE ( 'NONE', #5208, 10.00000000000000178 ) ;
#4062 = EDGE_LOOP ( 'NONE', ( #9056, #14926, #4927, #6454 ) ) ;
#4063 = CARTESIAN_POINT ( 'NONE',  ( 1.559999999999998943, 0.000000000000000000, 0.000000000000000000 ) ) ;
#4064 = LINE ( 'NONE', #7952, #14405 ) ;
#4065 = EDGE_CURVE ( 'NONE', #9320, #13341, #5617, .T. ) ;
#4066 = CARTESIAN_POINT ( 'NONE',  ( 27.75000000000000000, 2.516649172247811061E-16, -2.055000000000000160 ) ) ;
#4067 = SURFACE_STYLE_FILL_AREA ( #5397 ) ;
#4068 = CARTESIAN_POINT ( 'NONE',  ( 26.57417986947462651, 137.5626638350942699, -8.060801806284990434 ) ) ;
#4069 = ORIENTED_EDGE ( 'NONE', *, *, #5991, .T. ) ;
#4070 = CARTESIAN_POINT ( 'NONE',  ( -80.00000000000001421, 196.6227766016838245, 0.000000000000000000 ) ) ;
#4071 = CARTESIAN_POINT ( 'NONE',  ( -27.98221281347032274, 30.00000000000000000, 4.999999999999996447 ) ) ;
#4072 = ORIENTED_EDGE ( 'NONE', *, *, #10834, .F. ) ;
#4073 = CARTESIAN_POINT ( 'NONE',  ( 40.00000000000000711, 138.6227766016838245, -6.062001655779397722E-15 ) ) ;
#4074 = CARTESIAN_POINT ( 'NONE',  ( -74.09940879757193954, 195.3277913626825466, -25.76530748039454721 ) ) ;
#4075 = CARTESIAN_POINT ( 'NONE',  ( -18.25212770525997286, 32.30769230769230660, 4.999999999999999112 ) ) ;
#4076 = CARTESIAN_POINT ( 'NONE',  ( -80.00000000000001421, 196.6227766016838245, 11.50215154306610188 ) ) ;
#4077 = CARTESIAN_POINT ( 'NONE',  ( 28.15871609335591685, 18.00000000000000000, -20.05978710182010971 ) ) ;
#4078 = CARTESIAN_POINT ( 'NONE',  ( 21.38389869590601933, 18.00000000000114753, -9.948751090973035005 ) ) ;
#4079 = PLANE ( 'NONE',  #10369 ) ;
#4080 = DIRECTION ( 'NONE',  ( 1.000000000000000000, 0.000000000000000000, 0.000000000000000000 ) ) ;
#4081 = EDGE_CURVE ( 'NONE', #233, #2297, #533, .T. ) ;
#4082 = EDGE_CURVE ( 'NONE', #11435, #4527, #9271, .T. ) ;
#4083 = DIRECTION ( 'NONE',  ( 0.000000000000000000, 0.000000000000000000, 1.000000000000000000 ) ) ;
#4084 = ADVANCED_FACE ( 'NONE', ( #9178 ), #7676, .T. ) ;
#4085 = VECTOR ( 'NONE', #5468, 1000.000000000000000 ) ;
#4086 = VERTEX_POINT ( 'NONE', #5025 ) ;
#4087 = CARTESIAN_POINT ( 'NONE',  ( 48.00000000000000711, 159.6227766016838814, 3.071800142134975431 ) ) ;
#4088 = CIRCLE ( 'NONE', #17371, 5.000000000000018652 ) ;
#4089 = ORIENTED_EDGE ( 'NONE', *, *, #345, .F. ) ;
#4090 = CARTESIAN_POINT ( 'NONE',  ( -48.00000000000000000, 171.6227766016838245, 0.000000000000000000 ) ) ;
#4091 = DIRECTION ( 'NONE',  ( 0.000000000000000000, 0.000000000000000000, -1.000000000000000000 ) ) ;
#4092 = ORIENTED_EDGE ( 'NONE', *, *, #8714, .T. ) ;
#4093 = DIRECTION ( 'NONE',  ( 1.000000000000000000, 0.000000000000000000, -0.000000000000000000 ) ) ;
#4094 = CARTESIAN_POINT ( 'NONE',  ( 14.40174056114590151, 138.5906827818587885, 4.212836247846050597 ) ) ;
#4095 = ORIENTED_EDGE ( 'NONE', *, *, #2804, .T. ) ;
#4096 = CARTESIAN_POINT ( 'NONE',  ( 21.98114852961611376, 19.99999999999999645, 23.72829316725777460 ) ) ;
#4097 = VECTOR ( 'NONE', #11255, 1000.000000000000000 ) ;
#4098 = ORIENTED_EDGE ( 'NONE', *, *, #9339, .T. ) ;
#4099 = AXIS2_PLACEMENT_3D ( 'NONE', #16761, #1966, #1621 ) ;
#4100 = CARTESIAN_POINT ( 'NONE',  ( 196.0000000000000000, 171.6227766016838245, 15.00000337241049131 ) ) ;
#4101 = CARTESIAN_POINT ( 'NONE',  ( -40.00000000000000000, 4.000000000000000000, -33.00000000000000711 ) ) ;
#4102 = DIRECTION ( 'NONE',  ( -1.000000000000000000, -0.000000000000000000, -0.000000000000000000 ) ) ;
#4103 = CARTESIAN_POINT ( 'NONE',  ( -31.89848094669886436, 119.9728602285818084, -5.500000000000000000 ) ) ;
#4104 = EDGE_LOOP ( 'NONE', ( #16302, #4921, #7544, #8832 ) ) ;
#4105 = DIRECTION ( 'NONE',  ( -0.000000000000000000, -0.000000000000000000, -1.000000000000000000 ) ) ;
#4106 = ORIENTED_EDGE ( 'NONE', *, *, #16368, .T. ) ;
#4107 = CARTESIAN_POINT ( 'NONE',  ( -34.99999999999999289, 120.0000000000000284, 15.00000000000000000 ) ) ;
#4108 = DIRECTION ( 'NONE',  ( 1.000000000000000000, -0.000000000000000000, -0.000000000000000000 ) ) ;
#4109 = AXIS2_PLACEMENT_3D ( 'NONE', #1786, #9925, #16755 ) ;
#4110 = CARTESIAN_POINT ( 'NONE',  ( -5.000000000000000888, 206.6227766016838245, -2.143131898507868248E-15 ) ) ;
#4111 = ORIENTED_EDGE ( 'NONE', *, *, #13315, .F. ) ;
#4112 = ORIENTED_EDGE ( 'NONE', *, *, #13394, .T. ) ;
#4113 = FACE_OUTER_BOUND ( 'NONE', #12666, .T. ) ;
#4114 = ORIENTED_EDGE ( 'NONE', *, *, #1992, .F. ) ;
#4115 = DIRECTION ( 'NONE',  ( -0.000000000000000000, -0.000000000000000000, -1.000000000000000000 ) ) ;
#4116 = EDGE_CURVE ( 'NONE', #2623, #8731, #17243, .T. ) ;
#4117 = CARTESIAN_POINT ( 'NONE',  ( -32.66708739526796279, 119.0000000000000284, 4.722170599040653727 ) ) ;
#4118 = AXIS2_PLACEMENT_3D ( 'NONE', #13527, #3070, #9617 ) ;
#4119 = DIRECTION ( 'NONE',  ( -0.000000000000000000, -0.000000000000000000, -1.000000000000000000 ) ) ;
#4120 = CARTESIAN_POINT ( 'NONE',  ( -100.0000000000000000, 136.6227766016838245, 0.000000000000000000 ) ) ;
#4121 = CARTESIAN_POINT ( 'NONE',  ( -75.16806474348092593, 147.9395323639053856, 22.98372036160737153 ) ) ;
#4122 = AXIS2_PLACEMENT_3D ( 'NONE', #9711, #9626, #4240 ) ;
#4123 = ORIENTED_EDGE ( 'NONE', *, *, #1819, .T. ) ;
#4124 = CARTESIAN_POINT ( 'NONE',  ( -78.56757686808167307, 202.4505251070389704, -16.57269434321681345 ) ) ;
#4125 = CARTESIAN_POINT ( 'NONE',  ( 16.03791926353974162, 127.7299327228906520, 9.742640703122631862 ) ) ;
#4126 = FACE_OUTER_BOUND ( 'NONE', #10455, .T. ) ;
#4127 = CARTESIAN_POINT ( 'NONE',  ( -207.6770884633517653, 173.2520093125383198, 5.122071823546326286 ) ) ;
#4128 = CARTESIAN_POINT ( 'NONE',  ( -32.99999999999998579, 10.00000000000000000, -35.00200000000000244 ) ) ;
#4129 = EDGE_LOOP ( 'NONE', ( #4653, #5827 ) ) ;
#4130 = AXIS2_PLACEMENT_3D ( 'NONE', #15253, #6857, #297 ) ;
#4131 = AXIS2_PLACEMENT_3D ( 'NONE', #11182, #2063, #12864 ) ;
#4132 = CARTESIAN_POINT ( 'NONE',  ( 37.99999999999998579, 20.00000000000000000, -28.00000000000001066 ) ) ;
#4133 = CIRCLE ( 'NONE', #13177, 248.0000000000000000 ) ;
#4134 = ORIENTED_EDGE ( 'NONE', *, *, #7385, .F. ) ;
#4135 = CARTESIAN_POINT ( 'NONE',  ( 49.99999999999998579, 159.6227766016838814, -3.071800142134975431 ) ) ;
#4136 = ORIENTED_EDGE ( 'NONE', *, *, #9547, .F. ) ;
#4137 = FILL_AREA_STYLE_COLOUR ( '', #1345 ) ;
#4138 = CARTESIAN_POINT ( 'NONE',  ( 15.96677753504215858, 136.6227766016837961, -4.434194661153730915E-13 ) ) ;
#4139 = EDGE_CURVE ( 'NONE', #6006, #16523, #2365, .T. ) ;
#4140 = DIRECTION ( 'NONE',  ( -1.000000000000000000, -0.000000000000000000, -0.000000000000000000 ) ) ;
#4141 = DIRECTION ( 'NONE',  ( 1.000000000000000000, 0.000000000000000000, 0.000000000000000000 ) ) ;
#4142 = EDGE_CURVE ( 'NONE', #12705, #15849, #13301, .T. ) ;
#4143 = VECTOR ( 'NONE', #2844, 1000.000000000000000 ) ;
#4144 = VECTOR ( 'NONE', #1064, 1000.000000000000000 ) ;
#4145 = ORIENTED_EDGE ( 'NONE', *, *, #13237, .T. ) ;
#4146 = FACE_OUTER_BOUND ( 'NONE', #12831, .T. ) ;
#4147 = EDGE_CURVE ( 'NONE', #13207, #8108, #3069, .T. ) ;
#4148 = DIRECTION ( 'NONE',  ( -1.000000000000000000, 0.000000000000000000, 0.000000000000000000 ) ) ;
#4149 = PLANE ( 'NONE',  #4813 ) ;
#4150 = EDGE_CURVE ( 'NONE', #8931, #8731, #15999, .T. ) ;
#4151 = FACE_OUTER_BOUND ( 'NONE', #3309, .T. ) ;
#4152 = EDGE_CURVE ( 'NONE', #4664, #15793, #8244, .T. ) ;
#4153 = CARTESIAN_POINT ( 'NONE',  ( 14.43747245749253416, 129.4010981426196736, -11.63709869316310908 ) ) ;
#4154 = ORIENTED_EDGE ( 'NONE', *, *, #8876, .T. ) ;
#4155 = DIRECTION ( 'NONE',  ( -0.000000000000000000, -0.000000000000000000, -1.000000000000000000 ) ) ;
#4156 = CARTESIAN_POINT ( 'NONE',  ( 15.54198151645489645, 125.3641151175237667, -5.547502007357641318 ) ) ;
#4157 = VECTOR ( 'NONE', #1503, 1000.000000000000000 ) ;
#4158 = ORIENTED_EDGE ( 'NONE', *, *, #16909, .F. ) ;
#4159 = AXIS2_PLACEMENT_3D ( 'NONE', #11837, #11661, #10329 ) ;
#4160 = CARTESIAN_POINT ( 'NONE',  ( -81.12708499979228804, 190.7253031951458127, -29.32741221247050589 ) ) ;
#4161 = AXIS2_PLACEMENT_3D ( 'NONE', #17391, #929, #16072 ) ;
#4162 = CIRCLE ( 'NONE', #16875, 10.00000000000000000 ) ;
#4163 = CARTESIAN_POINT ( 'NONE',  ( 40.00000000000000000, 20.00000000000000000, 0.000000000000000000 ) ) ;
#4164 = CARTESIAN_POINT ( 'NONE',  ( 29.81269655378473971, 191.6224348813835263, 26.24906986711105716 ) ) ;
#4165 = CARTESIAN_POINT ( 'NONE',  ( 27.99999999999998224, 9.999999999999998224, -16.00000000000000000 ) ) ;
#4166 = CARTESIAN_POINT ( 'NONE',  ( 17.50698843878764777, 29.94827730614627725, -12.57924512168886011 ) ) ;
#4167 = DIRECTION ( 'NONE',  ( 0.000000000000000000, 0.000000000000000000, 1.000000000000000000 ) ) ;
#4168 = CARTESIAN_POINT ( 'NONE',  ( -22.99999999999998224, 10.00000000000000000, 35.00200000000000244 ) ) ;
#4169 = CARTESIAN_POINT ( 'NONE',  ( 39.99999999999999289, 8.000000000000000000, -39.99999999999999289 ) ) ;
#4170 = CARTESIAN_POINT ( 'NONE',  ( 26.52113164449903948, 141.7198527106616268, -18.19376952932830349 ) ) ;
#4171 = ORIENTED_EDGE ( 'NONE', *, *, #2170, .F. ) ;
#4172 = CARTESIAN_POINT ( 'NONE',  ( 9.103003883573421717, 133.2684780490642709, -14.60854014130129030 ) ) ;
#4173 = CIRCLE ( 'NONE', #4159, 5.000000000000006217 ) ;
#4174 = EDGE_LOOP ( 'NONE', ( #7685, #14413 ) ) ;
#4175 = DIRECTION ( 'NONE',  ( 1.000000000000000000, 0.000000000000000000, 0.000000000000000000 ) ) ;
#4176 = DIRECTION ( 'NONE',  ( 1.000000000000000000, -0.000000000000000000, -0.000000000000000000 ) ) ;
#4177 = ORIENTED_EDGE ( 'NONE', *, *, #8736, .F. ) ;
#4178 = CARTESIAN_POINT ( 'NONE',  ( -14.24512928960374225, 20.00000000000229505, 9.752520130898352235 ) ) ;
#4179 = CARTESIAN_POINT ( 'NONE',  ( 49.99999999999998579, 183.6227766016837961, -5.571800142134975431 ) ) ;
#4180 = EDGE_CURVE ( 'NONE', #14218, #233, #4215, .T. ) ;
#4181 = ORIENTED_EDGE ( 'NONE', *, *, #6754, .T. ) ;
#4182 = EDGE_CURVE ( 'NONE', #10541, #3188, #1096, .T. ) ;
#4183 = PRODUCT ( 'socket button head screw_iso_ISO 7380 - M5 x 25 - 25N', 'socket button head screw_iso_ISO 7380 - M5 x 25 - 25N', '', ( #11830 ) ) ;
#4184 = CARTESIAN_POINT ( 'NONE',  ( 28.86500048027878051, 154.0589040539455823, -27.93804624201380804 ) ) ;
#4185 = EDGE_CURVE ( 'NONE', #8740, #4376, #12395, .T. ) ;
#4186 = EDGE_LOOP ( 'NONE', ( #13901, #2845, #9933, #6077, #11937, #10823 ) ) ;
#4187 = CIRCLE ( 'NONE', #14351, 35.00000000000000000 ) ;
#4188 = DIRECTION ( 'NONE',  ( 1.000000000000000000, 0.000000000000000000, 0.000000000000000000 ) ) ;
#4189 = CARTESIAN_POINT ( 'NONE',  ( 36.80495063319472138, 193.4351830419513476, -24.76910924193870400 ) ) ;
#4190 = CARTESIAN_POINT ( 'NONE',  ( 40.00000000000000711, 138.6227766016838245, 6.062001655779397722E-15 ) ) ;
#4191 = EDGE_LOOP ( 'NONE', ( #12028, #9079, #5805 ) ) ;
#4192 = FACE_OUTER_BOUND ( 'NONE', #12058, .T. ) ;
#4193 = ORIENTED_EDGE ( 'NONE', *, *, #8859, .F. ) ;
#4194 = CARTESIAN_POINT ( 'NONE',  ( 27.58881406714485252, 151.0069623973649584, 25.76819119792229174 ) ) ;
#4195 = ORIENTED_EDGE ( 'NONE', *, *, #15421, .F. ) ;
#4196 = LINE ( 'NONE', #14987, #7598 ) ;
#4197 = FACE_OUTER_BOUND ( 'NONE', #7749, .T. ) ;
#4198 = CARTESIAN_POINT ( 'NONE',  ( -15.96992528024541613, 32.67167891243749978, -7.259156848219323166 ) ) ;
#4199 = VECTOR ( 'NONE', #1550, 1000.000000000000000 ) ;
#4200 = ORIENTED_EDGE ( 'NONE', *, *, #10540, .F. ) ;
#4201 = VERTEX_POINT ( 'NONE', #15021 ) ;
#4202 = EDGE_CURVE ( 'NONE', #118, #903, #8734, .T. ) ;
#4203 = EDGE_CURVE ( 'NONE', #3029, #15883, #5906, .T. ) ;
#4204 = CARTESIAN_POINT ( 'NONE',  ( -24.93725393319379435, 120.0000000000000284, -5.500000000000000000 ) ) ;
#4205 = B_SPLINE_CURVE_WITH_KNOTS ( 'NONE', 3,
 ( #8099, #12190, #1648, #10846, #16259, #4127, #9427, #13517, #9512, #8194, #15086, #229 ),
 .UNSPECIFIED., .F., .F.,
 ( 4, 2, 2, 2, 2, 4 ),
 ( 0.000000000000000000, 0.0006954760458706750904, 0.001390952091741350181, 0.001738690114676716024, 0.002086428137612082300, 0.002781904183482815287 ),
 .UNSPECIFIED. ) ;
#4206 = CARTESIAN_POINT ( 'NONE',  ( 49.99999999999998579, 191.6227766016837677, 5.571800142134975431 ) ) ;
#4207 = ORIENTED_EDGE ( 'NONE', *, *, #6451, .F. ) ;
#4208 = SHAPE_DEFINITION_REPRESENTATION ( #5739, #12790 ) ;
#4209 = DIRECTION ( 'NONE',  ( 0.000000000000000000, 0.000000000000000000, 1.000000000000000000 ) ) ;
#4210 = FACE_OUTER_BOUND ( 'NONE', #6693, .T. ) ;
#4211 = DIRECTION ( 'NONE',  ( 0.000000000000000000, 0.000000000000000000, -1.000000000000000000 ) ) ;
#4212 = DIRECTION ( 'NONE',  ( 0.000000000000000000, 0.000000000000000000, 1.000000000000000000 ) ) ;
#4213 = CARTESIAN_POINT ( 'NONE',  ( 17.00000000000000000, 154.3022685259950038, -9.999999999999900524 ) ) ;
#4214 = AXIS2_PLACEMENT_3D ( 'NONE', #9078, #6257, #10678 ) ;
#4215 = CIRCLE ( 'NONE', #3928, 2.000000000000001776 ) ;
#4216 = VERTEX_POINT ( 'NONE', #2724 ) ;
#4217 = FACE_OUTER_BOUND ( 'NONE', #1033, .T. ) ;
#4218 = CARTESIAN_POINT ( 'NONE',  ( 9.103003883573421717, 133.2684780490642709, 14.60854014130129030 ) ) ;
#4219 = DIRECTION ( 'NONE',  ( -0.000000000000000000, -0.000000000000000000, -1.000000000000000000 ) ) ;
#4220 = DIRECTION ( 'NONE',  ( 1.000000000000000000, 0.000000000000000000, 0.000000000000000000 ) ) ;
#4221 = PLANE ( 'NONE',  #5823 ) ;
#4222 = ORIENTED_EDGE ( 'NONE', *, *, #13115, .T. ) ;
#4223 = EDGE_CURVE ( 'NONE', #9434, #5867, #15502, .T. ) ;
#4224 = CIRCLE ( 'NONE', #1391, 33.00000000000000000 ) ;
#4225 = FACE_OUTER_BOUND ( 'NONE', #9263, .T. ) ;
#4226 = VECTOR ( 'NONE', #2777, 1000.000000000000000 ) ;
#4227 = VERTEX_POINT ( 'NONE', #7143 ) ;
#4228 = DIRECTION ( 'NONE',  ( 1.000000000000000000, 0.000000000000000000, 0.000000000000000000 ) ) ;
#4229 = AXIS2_PLACEMENT_3D ( 'NONE', #9572, #6667, #14891 ) ;
#4230 = EDGE_LOOP ( 'NONE', ( #15653, #6412, #3849, #13385 ) ) ;
#4231 = DIRECTION ( 'NONE',  ( 0.000000000000000000, -1.000000000000000000, -0.000000000000000000 ) ) ;
#4232 = DIRECTION ( 'NONE',  ( 0.000000000000000000, 0.000000000000000000, 1.000000000000000000 ) ) ;
#4233 = UNCERTAINTY_MEASURE_WITH_UNIT (LENGTH_MEASURE( 1.000000000000000082E-05 ), #5828, 'distance_accuracy_value', 'NONE');
#4234 = VERTEX_POINT ( 'NONE', #13696 ) ;
#4235 = FACE_OUTER_BOUND ( 'NONE', #17188, .T. ) ;
#4236 = VECTOR ( 'NONE', #1407, 1000.000000000000000 ) ;
#4237 = LINE ( 'NONE', #6973, #2544 ) ;
#4238 = DIRECTION ( 'NONE',  ( -0.7071067811865513475, 8.659560562354886020E-17, -0.7071067811865436870 ) ) ;
#4239 = AXIS2_PLACEMENT_3D ( 'NONE', #11072, #10987, #103 ) ;
#4240 = DIRECTION ( 'NONE',  ( 0.000000000000000000, 0.000000000000000000, 1.000000000000000000 ) ) ;
#4241 = ADVANCED_FACE ( 'NONE', ( #6968 ), #5338, .F. ) ;
#4242 = CARTESIAN_POINT ( 'NONE',  ( 16.17648631192976794, 127.5693673001539992, -9.524520547909567370 ) ) ;
#4243 = ORIENTED_EDGE ( 'NONE', *, *, #17126, .T. ) ;
#4244 = FACE_OUTER_BOUND ( 'NONE', #12879, .T. ) ;
#4245 = CARTESIAN_POINT ( 'NONE',  ( -68.00000000000000000, 154.3022685259950038, 9.999999999999900524 ) ) ;
#4246 = AXIS2_PLACEMENT_3D ( 'NONE', #6261, #11823, #14668 ) ;
#4247 = AXIS2_PLACEMENT_3D ( 'NONE', #3528, #11663, #6273 ) ;
#4248 = EDGE_LOOP ( 'NONE', ( #1288, #4456, #10497, #14437 ) ) ;
#4249 = CARTESIAN_POINT ( 'NONE',  ( -32.55406425504222057, 119.4745293701363664, -5.163900856529947347 ) ) ;
#4250 = EDGE_CURVE ( 'NONE', #6671, #17520, #17498, .T. ) ;
#4251 = CIRCLE ( 'NONE', #13300, 2.499999999999998668 ) ;
#4252 = EDGE_CURVE ( 'NONE', #5181, #2062, #16080, .T. ) ;
#4253 = DIRECTION ( 'NONE',  ( -1.000000000000000000, 0.000000000000000000, 0.000000000000000000 ) ) ;
#4254 = LINE ( 'NONE', #5667, #3875 ) ;
#4255 = DIRECTION ( 'NONE',  ( -0.000000000000000000, -0.000000000000000000, -1.000000000000000000 ) ) ;
#4256 = DIRECTION ( 'NONE',  ( 0.000000000000000000, 0.8660254037844363761, 0.5000000000000041078 ) ) ;
#4257 = EDGE_CURVE ( 'NONE', #2548, #5131, #11119, .T. ) ;
#4258 = CARTESIAN_POINT ( 'NONE',  ( 37.99999999999998579, 18.00000000000000355, -28.00000000000001066 ) ) ;
#4259 = CARTESIAN_POINT ( 'NONE',  ( 13.57836111649853450, 143.5532840108684525, -17.35359164609418059 ) ) ;
#4260 = DIRECTION ( 'NONE',  ( 0.000000000000000000, 0.000000000000000000, -1.000000000000000000 ) ) ;
#4261 = ORIENTED_EDGE ( 'NONE', *, *, #4986, .F. ) ;
#4262 = CARTESIAN_POINT ( 'NONE',  ( -14.90344812367259131, 20.00000000000343192, -8.058388986520416353 ) ) ;
#4263 = VECTOR ( 'NONE', #10494, 1000.000000000000114 ) ;
#4264 = ORIENTED_EDGE ( 'NONE', *, *, #14345, .F. ) ;
#4265 = CARTESIAN_POINT ( 'NONE',  ( 24.29786737972285238, 29.87659578631513568, -8.527395788633878482 ) ) ;
#4266 = CIRCLE ( 'NONE', #16433, 8.000000000000007105 ) ;
#4267 = DIRECTION ( 'NONE',  ( 0.000000000000000000, 0.000000000000000000, -1.000000000000000000 ) ) ;
#4268 = EDGE_LOOP ( 'NONE', ( #12681, #16145 ) ) ;
#4269 = CARTESIAN_POINT ( 'NONE',  ( -16.77496435665412733, 32.01311153724419967, 10.06041171812362300 ) ) ;
#4270 = CARTESIAN_POINT ( 'NONE',  ( 15.00000000000000000, 171.6227766016838245, -20.00000000000000355 ) ) ;
#4271 = ORIENTED_EDGE ( 'NONE', *, *, #4400, .T. ) ;
#4272 = CARTESIAN_POINT ( 'NONE',  ( 36.98037184620995532, 149.3990418665993047, -24.40116746791568758 ) ) ;
#4273 = EDGE_CURVE ( 'NONE', #793, #1279, #7586, .T. ) ;
#4274 = CIRCLE ( 'NONE', #16985, 5.000000000000004441 ) ;
#4275 = VERTEX_POINT ( 'NONE', #5467 ) ;
#4276 = CARTESIAN_POINT ( 'NONE',  ( -32.64269715136552463, 118.7804878048780779, -4.499999999999999112 ) ) ;
#4277 = DIRECTION ( 'NONE',  ( 1.000000000000000000, 0.000000000000000000, -0.000000000000000000 ) ) ;
#4278 = CARTESIAN_POINT ( 'NONE',  ( -725.0000000000001137, 129.9999999999995453, -4.999999999999999112 ) ) ;
#4279 = ORIENTED_EDGE ( 'NONE', *, *, #16848, .T. ) ;
#4280 = CARTESIAN_POINT ( 'NONE',  ( -100.0000000000000000, 120.0000000000000284, 6.000000000000001776 ) ) ;
#4281 = ORIENTED_EDGE ( 'NONE', *, *, #8513, .F. ) ;
#4282 = CARTESIAN_POINT ( 'NONE',  ( 12.82244027866276426, 141.9777490571136696, -18.60671400555900235 ) ) ;
#4283 = EDGE_CURVE ( 'NONE', #3210, #7915, #6759, .T. ) ;
#4284 = VERTEX_POINT ( 'NONE', #11037 ) ;
#4285 = CARTESIAN_POINT ( 'NONE',  ( -76.21324911630662768, 190.1432158455537262, -27.31345131271291038 ) ) ;
#4286 = CARTESIAN_POINT ( 'NONE',  ( -48.00000000000000000, 143.0439382767972347, 16.49999999999984368 ) ) ;
#4287 = AXIS2_PLACEMENT_3D ( 'NONE', #15608, #992, #9133 ) ;
#4288 = DIRECTION ( 'NONE',  ( 0.000000000000000000, 1.000000000000000000, 0.000000000000000000 ) ) ;
#4289 = VERTEX_POINT ( 'NONE', #407 ) ;
#4290 = ORIENTED_EDGE ( 'NONE', *, *, #2132, .F. ) ;
#4291 = LINE ( 'NONE', #1720, #9202 ) ;
#4292 = B_SPLINE_CURVE_WITH_KNOTS ( 'NONE', 3,
 ( #12147, #12400, #4344, #16401 ),
 .UNSPECIFIED., .F., .F.,
 ( 4, 4 ),
 ( 0.000000000000000000, 0.001170341053039947524 ),
 .UNSPECIFIED. ) ;
#4293 = CARTESIAN_POINT ( 'NONE',  ( -72.78662571002521986, 198.7412861714591088, -18.82352572523460310 ) ) ;
#4294 = CARTESIAN_POINT ( 'NONE',  ( 6.134011831684060390, 139.5514275721929209, 14.99999999999999822 ) ) ;
#4295 = VERTEX_POINT ( 'NONE', #12461 ) ;
#4296 = DIRECTION ( 'NONE',  ( -1.000000000000000000, -0.000000000000000000, -0.000000000000000000 ) ) ;
#4297 = CARTESIAN_POINT ( 'NONE',  ( -71.66708739526794147, 110.0000000000000142, 5.500000000000000000 ) ) ;
#4298 = DIRECTION ( 'NONE',  ( 0.000000000000000000, 0.000000000000000000, 1.000000000000000000 ) ) ;
#4299 = DIRECTION ( 'NONE',  ( -0.000000000000000000, -0.000000000000000000, 1.000000000000000000 ) ) ;
#4300 = CARTESIAN_POINT ( 'NONE',  ( 19.47274266584701508, 18.00000000000000000, 24.48069943974689266 ) ) ;
#4301 = ORIENTED_EDGE ( 'NONE', *, *, #1958, .F. ) ;
#4302 = FACE_OUTER_BOUND ( 'NONE', #3673, .T. ) ;
#4303 = EDGE_CURVE ( 'NONE', #5755, #2973, #16626, .T. ) ;
#4304 = EDGE_CURVE ( 'NONE', #7251, #16894, #5628, .T. ) ;
#4305 = DIRECTION ( 'NONE',  ( -1.000000000000000000, -0.000000000000000000, 0.000000000000000000 ) ) ;
#4306 = EDGE_CURVE ( 'NONE', #11681, #4396, #3639, .T. ) ;
#4307 = CARTESIAN_POINT ( 'NONE',  ( -25.00000000000000000, 120.0000000000000426, 10.85786437626905077 ) ) ;
#4308 = DIRECTION ( 'NONE',  ( -6.938893903907228378E-16, 1.000000000000000000, 0.000000000000000000 ) ) ;
#4309 = CARTESIAN_POINT ( 'NONE',  ( 35.00000000000000711, 146.6227766016838245, 21.54065922853802562 ) ) ;
#4310 = PRODUCT_DEFINITION_CONTEXT ( 'detailed design', #7096, 'design' ) ;
#4311 = ORIENTED_EDGE ( 'NONE', *, *, #2897, .T. ) ;
#4312 = EDGE_LOOP ( 'NONE', ( #5379, #62, #14990, #11609 ) ) ;
#4313 = DIRECTION ( 'NONE',  ( -0.000000000000000000, -0.000000000000000000, 1.000000000000000000 ) ) ;
#4314 = ORIENTED_EDGE ( 'NONE', *, *, #1484, .T. ) ;
#4315 = FACE_OUTER_BOUND ( 'NONE', #10906, .T. ) ;
#4316 = ORIENTED_EDGE ( 'NONE', *, *, #6851, .T. ) ;
#4317 = DIRECTION ( 'NONE',  ( 1.000000000000000000, -0.000000000000000000, -0.000000000000000000 ) ) ;
#4318 = CARTESIAN_POINT ( 'NONE',  ( -68.00000000000000000, 171.6227766016838245, 0.000000000000000000 ) ) ;
#4319 = DIRECTION ( 'NONE',  ( -1.000000000000000000, 0.000000000000000000, 0.000000000000000000 ) ) ;
#4320 = VERTEX_POINT ( 'NONE', #14300 ) ;
#4321 = DIRECTION ( 'NONE',  ( 0.000000000000000000, 0.000000000000000000, -1.000000000000000000 ) ) ;
#4322 = LINE ( 'NONE', #13700, #7340 ) ;
#4323 = CARTESIAN_POINT ( 'NONE',  ( -22.93725393319378369, 20.00000000000004263, 5.999999999999992895 ) ) ;
#4324 = CARTESIAN_POINT ( 'NONE',  ( -32.64269715136552463, 101.2195121951219647, -4.499999999999999112 ) ) ;
#4325 = PRODUCT_DEFINITION_SHAPE ( 'NONE', 'NONE',  #7612 ) ;
#4326 = CARTESIAN_POINT ( 'NONE',  ( 15.95013150516294154, 137.1612117474554111, -8.111885438162047990 ) ) ;
#4327 = VERTEX_POINT ( 'NONE', #15627 ) ;
#4328 = DIRECTION ( 'NONE',  ( -0.08715574274764828488, -0.4980973490458772135, 0.8627299156628193133 ) ) ;
#4329 = CARTESIAN_POINT ( 'NONE',  ( 13.90347339350139677, 138.7488974902626069, -3.510692536283880116 ) ) ;
#4330 = VERTEX_POINT ( 'NONE', #7320 ) ;
#4331 = CARTESIAN_POINT ( 'NONE',  ( -84.70068968583443336, 192.8887977548965296, -27.79913727548661839 ) ) ;
#4332 = DIRECTION ( 'NONE',  ( 0.000000000000000000, 0.000000000000000000, 1.000000000000000000 ) ) ;
#4333 = EDGE_CURVE ( 'NONE', #7814, #3299, #17204, .T. ) ;
#4334 = CARTESIAN_POINT ( 'NONE',  ( 29.61664150470813794, 191.6335950462332107, 26.24057872661396118 ) ) ;
#4335 = EDGE_CURVE ( 'NONE', #17412, #14332, #1945, .T. ) ;
#4336 = DIRECTION ( 'NONE',  ( -1.000000000000000000, 0.000000000000000000, 0.000000000000000000 ) ) ;
#4337 = DIRECTION ( 'NONE',  ( -1.000000000000000000, -0.000000000000000000, -0.000000000000000000 ) ) ;
#4338 = FACE_OUTER_BOUND ( 'NONE', #10292, .T. ) ;
#4339 = CARTESIAN_POINT ( 'NONE',  ( 9.156206820864191798, 144.1010407228830559, -18.21082046960973599 ) ) ;
#4340 = DIRECTION ( 'NONE',  ( 0.000000000000000000, 0.4999999999999997780, -0.8660254037844387076 ) ) ;
#4341 = ORIENTED_EDGE ( 'NONE', *, *, #11729, .F. ) ;
#4342 = ORIENTED_EDGE ( 'NONE', *, *, #4681, .T. ) ;
#4343 = DIRECTION ( 'NONE',  ( -0.000000000000000000, -0.000000000000000000, 1.000000000000000000 ) ) ;
#4344 = CARTESIAN_POINT ( 'NONE',  ( 15.39006516123636281, 143.0404737187717785, -16.50200026350847793 ) ) ;
#4345 = EDGE_LOOP ( 'NONE', ( #7028, #6429, #10102 ) ) ;
#4346 = PLANE ( 'NONE',  #8881 ) ;
#4347 = CARTESIAN_POINT ( 'NONE',  ( -103.0000000000000142, 171.6227766016838245, 0.000000000000000000 ) ) ;
#4348 = VERTEX_POINT ( 'NONE', #3243 ) ;
#4349 = CARTESIAN_POINT ( 'NONE',  ( 22.74938895237542624, 148.5880153409832189, -23.63707964515040061 ) ) ;
#4350 = FACE_OUTER_BOUND ( 'NONE', #2417, .T. ) ;
#4351 = CIRCLE ( 'NONE', #5653, 7.499999999999996447 ) ;
#4352 = EDGE_CURVE ( 'NONE', #9170, #3772, #1917, .T. ) ;
#4353 = CYLINDRICAL_SURFACE ( 'NONE', #8087, 19.49999999999998224 ) ;
#4354 = AXIS2_PLACEMENT_3D ( 'NONE', #4478, #3408, #2068 ) ;
#4355 = CARTESIAN_POINT ( 'NONE',  ( -5.000000000000000888, 191.6227766016837961, 1.224646799147353454E-15 ) ) ;
#4356 = DIRECTION ( 'NONE',  ( -0.000000000000000000, -0.000000000000000000, 1.000000000000000000 ) ) ;
#4357 = B_SPLINE_CURVE_WITH_KNOTS ( 'NONE', 3,
 ( #16408, #5506, #9831, #5685, #5853, #4272, #12314, #6912, #191, #15053, #16489, #4537, #11151, #12233, #15323, #12578, #9655, #8320, #8246, #7176, #2851, #10894, #11247, #13736, #1611, #16313, #4184, #16667, #4446, #9568, #7010, #8418, #12408, #3198, #5764, #12497, #14974, #13652, #8590, #4349, #9921, #1443, #6842, #9738, #15138, #3018 ),
 .UNSPECIFIED., .F., .F.,
 ( 4, 2, 2, 2, 2, 2, 2, 2, 2, 2, 2, 2, 2, 2, 2, 2, 2, 2, 2, 2, 2, 2, 4 ),
 ( 0.01035378412632265502, 0.01206629175607499757, 0.01377879938582734186, 0.01549130701557968615, 0.01634756083045588171, 0.01720381464533208074, 0.01806006846020827977, 0.01891632227508447534, 0.02062882990483680748, 0.02148508371971298223, 0.02234133753458915697, 0.02319759134946533172, 0.02405384516434150993, 0.02576635279409385942, 0.02747886042384620545, 0.02833511423872238019, 0.02919136805359855841, 0.03090387568335089402, 0.03261638331310323657, 0.03432889094285557913, 0.03604139857260792168, 0.03689765238748408949, 0.03775390620236026423 ),
 .UNSPECIFIED. ) ;
#4358 = DIRECTION ( 'NONE',  ( 0.000000000000000000, -1.000000000000000000, -8.673617379884035472E-17 ) ) ;
#4359 = DIRECTION ( 'NONE',  ( -1.000000000000000000, -0.000000000000000000, -0.000000000000000000 ) ) ;
#4360 = ORIENTED_EDGE ( 'NONE', *, *, #9371, .T. ) ;
#4361 = DIRECTION ( 'NONE',  ( 0.000000000000000000, 0.000000000000000000, -1.000000000000000000 ) ) ;
#4362 = ADVANCED_FACE ( 'NONE', ( #4584 ), #13550, .F. ) ;
#4363 = ORIENTED_EDGE ( 'NONE', *, *, #146, .F. ) ;
#4364 = ADVANCED_FACE ( 'NONE', ( #12726 ), #3426, .T. ) ;
#4365 = PLANE ( 'NONE',  #2243 ) ;
#4366 = DIRECTION ( 'NONE',  ( 1.000000000000000000, 0.000000000000000000, -0.000000000000000000 ) ) ;
#4367 = ADVANCED_FACE ( 'NONE', ( #12626 ), #11640, .T. ) ;
#4368 = LINE ( 'NONE', #4110, #7791 ) ;
#4369 = EDGE_LOOP ( 'NONE', ( #12572, #14160, #7511, #11246, #755, #6063 ) ) ;
#4370 = VERTEX_POINT ( 'NONE', #7480 ) ;
#4371 = LINE ( 'NONE', #9851, #1577 ) ;
#4372 = CIRCLE ( 'NONE', #5767, 7.500000000000000000 ) ;
#4373 = AXIS2_PLACEMENT_3D ( 'NONE', #14656, #6601, #11265 ) ;
#4374 = DIRECTION ( 'NONE',  ( -1.000000000000000000, 0.000000000000000000, 0.000000000000000000 ) ) ;
#4375 = CARTESIAN_POINT ( 'NONE',  ( 16.34705933256455879, 136.9208395216682561, 6.505922558274784606 ) ) ;
#4376 = VERTEX_POINT ( 'NONE', #678 ) ;
#4377 = EDGE_CURVE ( 'NONE', #3947, #15613, #9863, .T. ) ;
#4378 = CYLINDRICAL_SURFACE ( 'NONE', #28, 2.499999999999998668 ) ;
#4379 = DIRECTION ( 'NONE',  ( -0.000000000000000000, -0.000000000000000000, -1.000000000000000000 ) ) ;
#4380 = DIRECTION ( 'NONE',  ( 0.000000000000000000, 0.000000000000000000, 1.000000000000000000 ) ) ;
#4381 = CARTESIAN_POINT ( 'NONE',  ( 15.58935537591275811, 125.0306660307430349, 3.338448778865417577 ) ) ;
#4382 =( REPRESENTATION_RELATIONSHIP ('NONE','NONE', #9723, #17442 ) REPRESENTATION_RELATIONSHIP_WITH_TRANSFORMATION ( #5877 )SHAPE_REPRESENTATION_RELATIONSHIP( ) );
#4383 = CARTESIAN_POINT ( 'NONE',  ( 25.49876332522149625, 18.00000000000000000, 21.99427390110736624 ) ) ;
#4384 = CARTESIAN_POINT ( 'NONE',  ( 37.99999999999999289, 18.00000000000000355, -8.789265611615818404E-15 ) ) ;
#4385 = AXIS2_PLACEMENT_3D ( 'NONE', #15592, #3467, #8854 ) ;
#4386 = EDGE_LOOP ( 'NONE', ( #16515, #15678, #7445, #11296 ) ) ;
#4387 = DIRECTION ( 'NONE',  ( -0.000000000000000000, -0.000000000000000000, -1.000000000000000000 ) ) ;
#4389 = CYLINDRICAL_SURFACE ( 'NONE', #14442, 2.500000000000000444 ) ;
#4388 = AXIS2_PLACEMENT_3D ( 'NONE', #11350, #3026, #4628 ) ;
#4390 = CARTESIAN_POINT ( 'NONE',  ( 23.79315516583586643, 19.99999999999999645, -22.94240041036162836 ) ) ;
#4391 = CARTESIAN_POINT ( 'NONE',  ( 36.00000000000000711, 196.6227766016838245, -16.00000000000000000 ) ) ;
#4392 = CARTESIAN_POINT ( 'NONE',  ( 30.00000000000001066, 146.6227766016838245, -13.00000000000000000 ) ) ;
#4393 = VERTEX_POINT ( 'NONE', #11387 ) ;
#4394 = ORIENTED_EDGE ( 'NONE', *, *, #5331, .F. ) ;
#4395 = FACE_OUTER_BOUND ( 'NONE', #7602, .T. ) ;
#4396 = VERTEX_POINT ( 'NONE', #4661 ) ;
#4397 = DIRECTION ( 'NONE',  ( -0.08715574274765354457, -0.4980973490458646125, -0.8627299156628260857 ) ) ;
#4398 = AXIS2_PLACEMENT_3D ( 'NONE', #6846, #12236, #106 ) ;
#4399 = ORIENTED_EDGE ( 'NONE', *, *, #1255, .T. ) ;
#4400 = EDGE_CURVE ( 'NONE', #8669, #17476, #7878, .T. ) ;
#4401 =( NAMED_UNIT ( * ) SI_UNIT ( $, .STERADIAN. ) SOLID_ANGLE_UNIT ( ) );
#4402 = EDGE_CURVE ( 'NONE', #11461, #1227, #5065, .T. ) ;
#4403 = DIRECTION ( 'NONE',  ( 0.000000000000000000, 0.000000000000000000, -1.000000000000000000 ) ) ;
#4404 = PRESENTATION_LAYER_ASSIGNMENT (  '', '', ( #3829 ) ) ;
#4405 = ADVANCED_FACE ( 'NONE', ( #7406 ), #5642, .T. ) ;
#4406 = VECTOR ( 'NONE', #5909, 1000.000000000000000 ) ;
#4407 = DIRECTION ( 'NONE',  ( 0.000000000000000000, 0.000000000000000000, 1.000000000000000000 ) ) ;
#4408 = CARTESIAN_POINT ( 'NONE',  ( -206.8291083847463199, 166.6494249078165808, 0.6193335608963369543 ) ) ;
#4409 = CARTESIAN_POINT ( 'NONE',  ( -85.27494917608791525, 201.9542783778900059, -13.00000000000000000 ) ) ;
#4410 = ORIENTED_EDGE ( 'NONE', *, *, #11046, .T. ) ;
#4411 = CARTESIAN_POINT ( 'NONE',  ( 27.04340649081008507, 142.5787592618052599, 15.67196037041395940 ) ) ;
#4412 = CARTESIAN_POINT ( 'NONE',  ( 30.00000000000000355, 196.6227766016838245, 0.000000000000000000 ) ) ;
#4413 = LINE ( 'NONE', #14064, #13591 ) ;
#4414 = CARTESIAN_POINT ( 'NONE',  ( 37.99999999999999289, 18.00000000000000355, 0.000000000000000000 ) ) ;
#4415 = AXIS2_PLACEMENT_3D ( 'NONE', #13143, #10390, #5003 ) ;
#4416 = VECTOR ( 'NONE', #10930, 1000.000000000000000 ) ;
#4417 =( BOUNDED_CURVE ( )  B_SPLINE_CURVE ( 3, ( #9196, #6639, #739, #9379 ),
 .UNSPECIFIED., .F., .F. ) 
 B_SPLINE_CURVE_WITH_KNOTS ( ( 4, 4 ),
 ( 0.000000000000000000, 1.490556265852237994 ),
 .UNSPECIFIED. ) 
 CURVE ( )  GEOMETRIC_REPRESENTATION_ITEM ( )  RATIONAL_B_SPLINE_CURVE ( ( 1.000000000000000000, 0.8232662051119113977, 0.8232662051119113977, 1.000000000000000000 ) ) 
 REPRESENTATION_ITEM ( '' )  );
#4418 = CARTESIAN_POINT ( 'NONE',  ( -95.00000000000000000, 141.6227766016838245, 5.510910596163088767E-15 ) ) ;
#4419 = VERTEX_POINT ( 'NONE', #17045 ) ;
#4420 = DIRECTION ( 'NONE',  ( 1.000000000000000000, 0.000000000000000000, 0.000000000000000000 ) ) ;
#4421 = VERTEX_POINT ( 'NONE', #5908 ) ;
#4422 = ADVANCED_FACE ( 'NONE', ( #10229 ), #3504, .T. ) ;
#4423 = DIRECTION ( 'NONE',  ( -1.000000000000000000, 0.000000000000000000, 0.000000000000000000 ) ) ;
#4424 = VECTOR ( 'NONE', #16501, 1000.000000000000000 ) ;
#4425 = VECTOR ( 'NONE', #10207, 1000.000000000000000 ) ;
#4426 = DIRECTION ( 'NONE',  ( 0.000000000000000000, 0.000000000000000000, -1.000000000000000000 ) ) ;
#4427 = AXIS2_PLACEMENT_3D ( 'NONE', #6238, #5893, #12968 ) ;
#4428 = DIRECTION ( 'NONE',  ( 1.000000000000000000, 0.000000000000000000, 0.000000000000000000 ) ) ;
#4429 = CARTESIAN_POINT ( 'NONE',  ( 22.99999999999997868, 9.999999999999998224, -35.00200000000000244 ) ) ;
#4430 = LINE ( 'NONE', #2916, #16036 ) ;
#4431 = CARTESIAN_POINT ( 'NONE',  ( 22.88339857903067198, 29.84310082762161187, 6.047897139192784266 ) ) ;
#4432 = CARTESIAN_POINT ( 'NONE',  ( -84.47031951572937203, 198.8808217108462770, 18.60648811928366442 ) ) ;
#4433 = CARTESIAN_POINT ( 'NONE',  ( -80.00000000000002842, 146.6227766016838245, 11.50215154306610188 ) ) ;
#4434 = VERTEX_POINT ( 'NONE', #6074 ) ;
#4435 = EDGE_LOOP ( 'NONE', ( #9208, #8069, #14147, #3246, #3176, #5592, #2473, #8334, #15358 ) ) ;
#4436 = LINE ( 'NONE', #8583, #2977 ) ;
#4437 = CIRCLE ( 'NONE', #13184, 23.61711149033412127 ) ;
#4438 = VECTOR ( 'NONE', #9203, 1000.000000000000000 ) ;
#4439 = DIRECTION ( 'NONE',  ( 1.000000000000000000, 0.000000000000000000, 0.000000000000000000 ) ) ;
#4440 = ORIENTED_EDGE ( 'NONE', *, *, #7209, .T. ) ;
#4441 = EDGE_CURVE ( 'NONE', #11986, #15706, #252, .T. ) ;
#4442 = CARTESIAN_POINT ( 'NONE',  ( -24.81085081035532269, 19.99999999999999645, 15.69149817756037457 ) ) ;
#4443 = AXIS2_PLACEMENT_3D ( 'NONE', #7333, #10240, #7156 ) ;
#4444 = FACE_OUTER_BOUND ( 'NONE', #9576, .T. ) ;
#4445 = ORIENTED_EDGE ( 'NONE', *, *, #17458, .F. ) ;
#4446 = CARTESIAN_POINT ( 'NONE',  ( 27.20631483639104076, 153.6052450214444889, -27.64877209012308512 ) ) ;
#4447 = CARTESIAN_POINT ( 'NONE',  ( -24.80114670877659222, 18.00000000000000000, 15.70637264050927051 ) ) ;
#4448 = CARTESIAN_POINT ( 'NONE',  ( -206.3689767832464668, 166.7044760491588704, -0.5444864983988328966 ) ) ;
#4449 = DIRECTION ( 'NONE',  ( -0.08715574274765354457, -0.4980973490458646125, -0.8627299156628260857 ) ) ;
#4450 = FACE_OUTER_BOUND ( 'NONE', #1831, .T. ) ;
#4451 = TOROIDAL_SURFACE ( 'NONE', #2460, 740.0000000000000000, 8.000000000000000000 ) ;
#4452 = CARTESIAN_POINT ( 'NONE',  ( -32.66708739526796279, 119.0000000000000284, 4.722170599040653727 ) ) ;
#4453 = MECHANICAL_DESIGN_GEOMETRIC_PRESENTATION_REPRESENTATION (  '', ( #10112 ), #3313 ) ;
#4454 = VECTOR ( 'NONE', #12364, 1000.000000000000000 ) ;
#4455 = DIRECTION ( 'NONE',  ( 0.000000000000000000, -1.000000000000000000, 6.123233995736762338E-17 ) ) ;
#4456 = ORIENTED_EDGE ( 'NONE', *, *, #5294, .T. ) ;
#4457 = CARTESIAN_POINT ( 'NONE',  ( 15.72080254704531477, 141.4281235329943343, -17.70852598599439176 ) ) ;
#4458 = ORIENTED_EDGE ( 'NONE', *, *, #6526, .T. ) ;
#4459 = LINE ( 'NONE', #3300, #12407 ) ;
#4460 = CARTESIAN_POINT ( 'NONE',  ( 0.000000000000000000, 18.00000000000000355, 0.000000000000000000 ) ) ;
#4461 = ORIENTED_EDGE ( 'NONE', *, *, #3539, .T. ) ;
#4462 = VERTEX_POINT ( 'NONE', #15289 ) ;
#4463 = EDGE_CURVE ( 'NONE', #6774, #3061, #16668, .T. ) ;
#4464 = DIRECTION ( 'NONE',  ( 1.000000000000000000, 0.000000000000000000, 0.000000000000000000 ) ) ;
#4465 = CIRCLE ( 'NONE', #15476, 2.500000000000000000 ) ;
#4466 = DIRECTION ( 'NONE',  ( 8.673617379884037937E-17, 0.000000000000000000, -1.000000000000000000 ) ) ;
#4467 = CARTESIAN_POINT ( 'NONE',  ( 16.17648631192976794, 127.5693673001539992, 9.524520547909567370 ) ) ;
#4468 = AXIS2_PLACEMENT_3D ( 'NONE', #2653, #10612, #7452 ) ;
#4469 = ORIENTED_EDGE ( 'NONE', *, *, #15780, .F. ) ;
#4470 = CARTESIAN_POINT ( 'NONE',  ( -34.99999999999999289, 130.0000000000000000, 0.000000000000000000 ) ) ;
#4471 = EDGE_CURVE ( 'NONE', #12970, #4801, #2261, .T. ) ;
#4472 = CARTESIAN_POINT ( 'NONE',  ( -96.00000000000001421, 171.6227766016838245, 0.000000000000000000 ) ) ;
#4473 = EDGE_CURVE ( 'NONE', #3234, #17055, #6772, .T. ) ;
#4474 = CARTESIAN_POINT ( 'NONE',  ( -84.53371403557255803, 194.4926179048318318, 23.79294127240568457 ) ) ;
#4475 = CARTESIAN_POINT ( 'NONE',  ( -31.66708739526795924, 101.0000000000000142, 5.500000000000000000 ) ) ;
#4476 = CARTESIAN_POINT ( 'NONE',  ( 15.45450437963097912, 29.98942126207016301, 13.00000000000000178 ) ) ;
#4477 = PRODUCT_DEFINITION_SHAPE ( 'NONE', 'NONE',  #5120 ) ;
#4478 = CARTESIAN_POINT ( 'NONE',  ( -95.00000000000000000, 171.6227766016838245, 0.000000000000000000 ) ) ;
#4479 = ORIENTED_EDGE ( 'NONE', *, *, #9881, .T. ) ;
#4480 = CARTESIAN_POINT ( 'NONE',  ( -74.16379527187788767, 198.0598900292995097, -22.94241666008129243 ) ) ;
#4481 = CARTESIAN_POINT ( 'NONE',  ( -86.00000000000001421, 196.6227766016838245, -16.00000000000000000 ) ) ;
#4482 = LINE ( 'NONE', #6952, #6475 ) ;
#4483 = DIRECTION ( 'NONE',  ( -1.156482317317868274E-16, 1.000000000000000000, 0.000000000000000000 ) ) ;
#4484 = CIRCLE ( 'NONE', #12381, 5.000000000000000888 ) ;
#4485 = CARTESIAN_POINT ( 'NONE',  ( -80.00000000000001421, 196.6227766016838245, -35.00200000000000244 ) ) ;
#4486 = ORIENTED_EDGE ( 'NONE', *, *, #3930, .T. ) ;
#4487 = VERTEX_POINT ( 'NONE', #1014 ) ;
#4488 = CARTESIAN_POINT ( 'NONE',  ( 7.535032041484082121, 144.1839557648053187, 18.33333333253072794 ) ) ;
#4489 = VERTEX_POINT ( 'NONE', #2343 ) ;
#4490 = FACE_OUTER_BOUND ( 'NONE', #15698, .T. ) ;
#4491 = PRODUCT_DEFINITION ( 'UNKNOWN', '', #9255, #8364 ) ;
#4492 = ORIENTED_EDGE ( 'NONE', *, *, #15369, .F. ) ;
#4493 =( LENGTH_UNIT ( ) NAMED_UNIT ( * ) SI_UNIT ( .MILLI., .METRE. ) );
#4494 = FACE_OUTER_BOUND ( 'NONE', #8956, .T. ) ;
#4495 = AXIS2_PLACEMENT_3D ( 'NONE', #2979, #9699, #10855 ) ;
#4496 = CARTESIAN_POINT ( 'NONE',  ( -207.5170152892447675, 166.4407316555380589, 0.9960724843441398635 ) ) ;
#4497 = FACE_OUTER_BOUND ( 'NONE', #9359, .T. ) ;
#4498 = ORIENTED_EDGE ( 'NONE', *, *, #1705, .F. ) ;
#4499 = CARTESIAN_POINT ( 'NONE',  ( 196.0000000000000000, 167.6227766016838814, -21.92820660268601074 ) ) ;
#4500 = DIRECTION ( 'NONE',  ( 0.000000000000000000, 0.000000000000000000, 1.000000000000000000 ) ) ;
#4501 = CARTESIAN_POINT ( 'NONE',  ( -7.379000772445021283, 18.00000000000000000, 25.00000000000000355 ) ) ;
#4502 = CARTESIAN_POINT ( 'NONE',  ( 25.00000000000000000, 196.6227766016838245, 35.00200000000000244 ) ) ;
#4503 = TOROIDAL_SURFACE ( 'NONE', #9008, 740.0000000000000000, 10.00000000000000000 ) ;
#4504 = EDGE_CURVE ( 'NONE', #16539, #11464, #6554, .T. ) ;
#4505 = VECTOR ( 'NONE', #5178, 1000.000000000000000 ) ;
#4506 = DIRECTION ( 'NONE',  ( 0.000000000000000000, -1.000000000000000000, 6.123233995736762338E-17 ) ) ;
#4507 = ORIENTED_EDGE ( 'NONE', *, *, #7212, .F. ) ;
#4508 = CARTESIAN_POINT ( 'NONE',  ( -71.66708739526794147, 110.0000000000000142, -5.500000000000000000 ) ) ;
#4509 = EDGE_LOOP ( 'NONE', ( #12223, #8545, #2346, #12909 ) ) ;
#4510 = SURFACE_STYLE_FILL_AREA ( #9543 ) ;
#4511 = CARTESIAN_POINT ( 'NONE',  ( 27.19159743497788284, 137.1791639268274992, 6.327035192214271575 ) ) ;
#4512 = CARTESIAN_POINT ( 'NONE',  ( 30.00000000000001066, 146.6227766016838245, -16.00000000000000000 ) ) ;
#4513 = CIRCLE ( 'NONE', #12714, 33.00000000000000000 ) ;
#4514 = AXIS2_PLACEMENT_3D ( 'NONE', #8788, #5059, #15676 ) ;
#4515 = CARTESIAN_POINT ( 'NONE',  ( -68.00000000000000000, 171.6227766016838245, 0.000000000000000000 ) ) ;
#4516 = VECTOR ( 'NONE', #8440, 1000.000000000000000 ) ;
#4517 = LINE ( 'NONE', #4429, #9999 ) ;
#4518 = LINE ( 'NONE', #11232, #7823 ) ;
#4519 = CARTESIAN_POINT ( 'NONE',  ( 18.93858299686282365, 29.91990340250987757, 11.93041869825017898 ) ) ;
#4520 = LINE ( 'NONE', #7425, #10177 ) ;
#4521 = DIRECTION ( 'NONE',  ( 0.000000000000000000, 0.000000000000000000, 1.000000000000000000 ) ) ;
#4522 = EDGE_LOOP ( 'NONE', ( #13245, #15418, #16764, #6931 ) ) ;
#4523 =( BOUNDED_SURFACE ( )  B_SPLINE_SURFACE ( 3, 2, ( 
 ( #479, #16695, #4564 ),
 ( #14035, #9949, #3224 ),
 ( #4644, #15439, #11974 ),
 ( #17029, #3570, #15877 ),
 ( #918, #2326, #993 ),
 ( #8964, #16057, #2509 ),
 ( #7718, #6491, #13128 ),
 ( #3838, #10550, #2244 ),
 ( #6669, #7905, #6305 ),
 ( #6397, #11697, #17109 ),
 ( #5073, #14636, #9318 ),
 ( #11792, #4982, #9228 ),
 ( #1089, #2604, #10285 ),
 ( #14541, #7810, #11885 ),
 ( #9134, #17197, #10472 ),
 ( #15686, #1179, #4894 ),
 ( #5164, #17294, #13048 ),
 ( #3934, #3747, #14730 ),
 ( #10650, #7990, #13396 ),
 ( #13314, #2412, #10373 ),
 ( #14460, #5245, #13220 ),
 ( #15958, #1264, #14375 ),
 ( #6583, #15784, #17375 ),
 ( #7637, #3666, #9055 ) ),
 .UNSPECIFIED., .F., .F., .F. ) 
 B_SPLINE_SURFACE_WITH_KNOTS ( ( 4, 2, 2, 2, 2, 2, 2, 2, 2, 2, 2, 4 ),
 ( 3, 3 ),
 ( 0.01427588378380421734, 0.01824401167166928364, 0.02022807561560181766, 0.02221213955953435168, 0.02618026744739941625, 0.02816433139133195027, 0.03014839533526448428, 0.03411652322312955232, 0.03610058716706208287, 0.03808465111099461342, 0.04205277899885968146, 0.04602090688672474950 ),
 ( 0.000000000000000000, 1.000000000000000000 ),
 .UNSPECIFIED. ) 
 GEOMETRIC_REPRESENTATION_ITEM ( )  RATIONAL_B_SPLINE_SURFACE ( (
 ( 1.000000000000000000, 0.7071067811865476838, 1.000000000000000000),
 ( 1.000000000000000000, 0.7013659285812973154, 1.000000000000000000),
 ( 1.000000000000000000, 0.6957352470445186121, 1.000000000000000000),
 ( 1.000000000000000000, 0.6874449304734518984, 1.000000000000000000),
 ( 1.000000000000000000, 0.6847075230360146758, 1.000000000000000000),
 ( 1.000000000000000000, 0.6792848743381181276, 1.000000000000000000),
 ( 1.000000000000000000, 0.6765866164120997173, 1.000000000000000000),
 ( 1.000000000000000000, 0.6687223666255138754, 1.000000000000000000),
 ( 1.000000000000000000, 0.6637534122519734847, 1.000000000000000000),
 ( 1.000000000000000000, 0.6567012635109988894, 1.000000000000000000),
 ( 1.000000000000000000, 0.6544178910916050862, 1.000000000000000000),
 ( 1.000000000000000000, 0.6499901663948596253, 1.000000000000000000),
 ( 1.000000000000000000, 0.6478648508490586488, 1.000000000000000000),
 ( 1.000000000000000000, 0.6418284244075036504, 1.000000000000000000),
 ( 1.000000000000000000, 0.6382188548936987837, 1.000000000000000000),
 ( 1.000000000000000000, 0.6334349500989925330, 1.000000000000000000),
 ( 1.000000000000000000, 0.6319385063093012622, 1.000000000000000000),
 ( 1.000000000000000000, 0.6292162870120669993, 1.000000000000000000),
 ( 1.000000000000000000, 0.6279881568153810045, 1.000000000000000000),
 ( 1.000000000000000000, 0.6246939197237914021, 1.000000000000000000),
 ( 1.000000000000000000, 0.6230139244306683866, 1.000000000000000000),
 ( 1.000000000000000000, 0.6207349535630238835, 1.000000000000000000),
 ( 1.000000000000000000, 0.6201739322038456459, 1.000000000000000000),
 ( 1.000000000000000000, 0.6201736729460424202, 1.000000000000000000) ) ) 
 REPRESENTATION_ITEM ( '' )  SURFACE ( )  );
#4524 = EDGE_CURVE ( 'NONE', #6195, #14777, #3379, .T. ) ;
#4525 = EDGE_CURVE ( 'NONE', #4801, #4546, #3763, .T. ) ;
#4526 = EDGE_CURVE ( 'NONE', #12455, #12513, #10569, .T. ) ;
#4527 = VERTEX_POINT ( 'NONE', #50 ) ;
#4528 = CARTESIAN_POINT ( 'NONE',  ( 34.93420767853318409, 19.99999999999999645, -5.000000000000010658 ) ) ;
#4529 = ADVANCED_FACE ( 'NONE', ( #5451 ), #11558, .F. ) ;
#4530 = AXIS2_PLACEMENT_3D ( 'NONE', #12495, #11149, #9829 ) ;
#4531 = CARTESIAN_POINT ( 'NONE',  ( 26.66247177481912800, 139.4607352144954007, -7.398570892697257761 ) ) ;
#4532 = ORIENTED_EDGE ( 'NONE', *, *, #5052, .T. ) ;
#4533 = CARTESIAN_POINT ( 'NONE',  ( 196.0000000000000000, 159.6227766016838814, -5.571800142134975431 ) ) ;
#4534 = CIRCLE ( 'NONE', #13581, 20.00000000000000355 ) ;
#4535 = CARTESIAN_POINT ( 'NONE',  ( 1.559999999999998943, -1.732050807568885631, 0.000000000000000000 ) ) ;
#4536 = ORIENTED_EDGE ( 'NONE', *, *, #16829, .T. ) ;
#4537 = CARTESIAN_POINT ( 'NONE',  ( 35.62055130997416796, 151.5947363889490589, -26.22852547856964378 ) ) ;
#4538 = CARTESIAN_POINT ( 'NONE',  ( -11.98734322101359240, 18.00000000000000355, 24.50584837321702736 ) ) ;
#4539 = DIRECTION ( 'NONE',  ( 0.000000000000000000, 0.000000000000000000, 1.000000000000000000 ) ) ;
#4540 = DIRECTION ( 'NONE',  ( 1.000000000000000000, -0.000000000000000000, -0.000000000000000000 ) ) ;
#4541 = CIRCLE ( 'NONE', #5390, 110.0000000000000142 ) ;
#4542 = FACE_OUTER_BOUND ( 'NONE', #13861, .T. ) ;
#4543 = LINE ( 'NONE', #9929, #5507 ) ;
#4544 = ADVANCED_FACE ( 'NONE', ( #1545 ), #2793, .F. ) ;
#4545 = CARTESIAN_POINT ( 'NONE',  ( -74.10793207926305115, 141.9594008680238062, -14.48313018527311868 ) ) ;
#4546 = VERTEX_POINT ( 'NONE', #16438 ) ;
#4547 = DIRECTION ( 'NONE',  ( 0.000000000000000000, 0.000000000000000000, -1.000000000000000000 ) ) ;
#4548 = ORIENTED_EDGE ( 'NONE', *, *, #10556, .T. ) ;
#4549 = PLANE ( 'NONE',  #3651 ) ;
#4550 = CARTESIAN_POINT ( 'NONE',  ( -24.99999999999999289, 90.00000000000000000, 15.00000000000000000 ) ) ;
#4551 = VERTEX_POINT ( 'NONE', #10760 ) ;
#4552 = DIRECTION ( 'NONE',  ( -1.000000000000000000, -0.000000000000000000, 0.000000000000000000 ) ) ;
#4553 = AXIS2_PLACEMENT_3D ( 'NONE', #7129, #12528, #393 ) ;
#4554 = CARTESIAN_POINT ( 'NONE',  ( 27.47046887371370616, 136.6950068244141221, 2.596529902249163690 ) ) ;
#4555 = CARTESIAN_POINT ( 'NONE',  ( 26.13287303778632165, 137.8093815885048627, 9.050576676228219597 ) ) ;
#4556 = AXIS2_PLACEMENT_3D ( 'NONE', #17489, #2872, #8267 ) ;
#4557 = ORIENTED_EDGE ( 'NONE', *, *, #13622, .F. ) ;
#4558 = DIRECTION ( 'NONE',  ( 0.000000000000000000, 1.000000000000000000, 0.000000000000000000 ) ) ;
#4559 = LINE ( 'NONE', #11274, #441 ) ;
#4560 = CARTESIAN_POINT ( 'NONE',  ( 30.00000000000001066, 146.6227766016838245, -35.00000000000000000 ) ) ;
#4561 = CARTESIAN_POINT ( 'NONE',  ( -3.000000000000000888, 171.6227766016838245, -20.00000000000000355 ) ) ;
#4562 = ADVANCED_FACE ( 'NONE', ( #8184 ), #4043, .T. ) ;
#4563 = CARTESIAN_POINT ( 'NONE',  ( 19.16009641331746849, 29.91553747150882359, 11.79770956048753838 ) ) ;
#4564 = CARTESIAN_POINT ( 'NONE',  ( -7.379000772444995526, 18.00000000000000000, -25.00000000000000000 ) ) ;
#4565 = EDGE_CURVE ( 'NONE', #6476, #16806, #9012, .T. ) ;
#4566 = VERTEX_POINT ( 'NONE', #16343 ) ;
#4567 = DIRECTION ( 'NONE',  ( -0.000000000000000000, -0.000000000000000000, 1.000000000000000000 ) ) ;
#4568 = AXIS2_PLACEMENT_3D ( 'NONE', #13657, #2508, #14807 ) ;
#4569 = DIRECTION ( 'NONE',  ( 0.000000000000000000, -1.000000000000000000, -6.123233995736762338E-17 ) ) ;
#4570 = ORIENTED_EDGE ( 'NONE', *, *, #14637, .F. ) ;
#4571 = PLANE ( 'NONE',  #10997 ) ;
#4572 = CARTESIAN_POINT ( 'NONE',  ( 50.00000000000000000, 171.6227766016838245, 0.000000000000000000 ) ) ;
#4573 = ORIENTED_EDGE ( 'NONE', *, *, #5497, .F. ) ;
#4574 = ORIENTED_EDGE ( 'NONE', *, *, #15169, .T. ) ;
#4575 = ORIENTED_EDGE ( 'NONE', *, *, #15298, .T. ) ;
#4576 = EDGE_CURVE ( 'NONE', #4327, #12781, #14914, .T. ) ;
#4577 = CARTESIAN_POINT ( 'NONE',  ( 12.89436750745977989, 143.6582566230365501, 17.52127501928458031 ) ) ;
#4578 = ORIENTED_EDGE ( 'NONE', *, *, #12564, .T. ) ;
#4579 = CARTESIAN_POINT ( 'NONE',  ( -68.00000000000000000, 171.6227766016838245, 0.000000000000000000 ) ) ;
#4580 = VECTOR ( 'NONE', #5769, 1000.000000000000000 ) ;
#4581 = VERTEX_POINT ( 'NONE', #5366 ) ;
#4582 = DIRECTION ( 'NONE',  ( -1.000000000000000000, 0.000000000000000000, 0.000000000000000000 ) ) ;
#4583 = CYLINDRICAL_SURFACE ( 'NONE', #12311, 2.500000000000000444 ) ;
#4584 = FACE_OUTER_BOUND ( 'NONE', #16122, .T. ) ;
#4585 = LINE ( 'NONE', #2013, #11175 ) ;
#4586 = VERTEX_POINT ( 'NONE', #9419 ) ;
#4587 = CARTESIAN_POINT ( 'NONE',  ( 25.98421795186086314, 143.6297497249236130, 17.48070775079459338 ) ) ;
#4588 = DIRECTION ( 'NONE',  ( -0.01578383822436034076, 0.1110972697184772484, -0.9936841888205766304 ) ) ;
#4589 = LINE ( 'NONE', #9969, #9050 ) ;
#4590 = CARTESIAN_POINT ( 'NONE',  ( -12.77984573873758656, 20.00000000000345679, -11.87289823213939854 ) ) ;
#4591 = CARTESIAN_POINT ( 'NONE',  ( 14.93242934743710393, 30.00000000000000000, 25.00000000000000000 ) ) ;
#4592 = EDGE_CURVE ( 'NONE', #16329, #2257, #7793, .T. ) ;
#4593 = EDGE_CURVE ( 'NONE', #16788, #11875, #17511, .T. ) ;
#4594 = FACE_OUTER_BOUND ( 'NONE', #16314, .T. ) ;
#4595 = VERTEX_POINT ( 'NONE', #2874 ) ;
#4596 = DIRECTION ( 'NONE',  ( 0.000000000000000000, 0.000000000000000000, 1.000000000000000000 ) ) ;
#4597 = ORIENTED_EDGE ( 'NONE', *, *, #9264, .F. ) ;
#4598 = APPLICATION_PROTOCOL_DEFINITION ( 'draft international standard', 'automotive_design', 1998, #10363 ) ;
#4599 = CARTESIAN_POINT ( 'NONE',  ( -86.00000000000001421, 196.6227766016838245, -24.49489742783178770 ) ) ;
#4600 = EDGE_LOOP ( 'NONE', ( #5693, #2635 ) ) ;
#4601 = CARTESIAN_POINT ( 'NONE',  ( 49.99999999999998579, 155.6227766016839098, -12.50000337241049309 ) ) ;
#4602 = ADVANCED_FACE ( 'NONE', ( #9769 ), #1378, .T. ) ;
#4603 = CARTESIAN_POINT ( 'NONE',  ( 37.99999999999998579, 18.00000000000000355, 28.00000000000001066 ) ) ;
#4604 = ORIENTED_EDGE ( 'NONE', *, *, #2930, .F. ) ;
#4605 = LINE ( 'NONE', #10076, #10933 ) ;
#4606 = CARTESIAN_POINT ( 'NONE',  ( 1.559999999999998943, 0.8660254037844428154, -1.499999999999997780 ) ) ;
#4607 = CARTESIAN_POINT ( 'NONE',  ( -84.88899566805817187, 197.8164829328480891, 20.09296681051160149 ) ) ;
#4608 = FACE_BOUND ( 'NONE', #11129, .T. ) ;
#4609 = VERTEX_POINT ( 'NONE', #12181 ) ;
#4610 = ORIENTED_EDGE ( 'NONE', *, *, #2804, .F. ) ;
#4611 = CARTESIAN_POINT ( 'NONE',  ( 24.87018239537452757, 29.86925179676151032, -6.310755877675157777 ) ) ;
#4612 = CARTESIAN_POINT ( 'NONE',  ( 20.85969470496125666, 141.7883037112096929, -14.11015612222007398 ) ) ;
#4613 = ORIENTED_EDGE ( 'NONE', *, *, #12667, .F. ) ;
#4614 = DIRECTION ( 'NONE',  ( -0.000000000000000000, -0.000000000000000000, -1.000000000000000000 ) ) ;
#4615 = DIRECTION ( 'NONE',  ( 1.000000000000000000, -0.000000000000000000, -0.000000000000000000 ) ) ;
#4616 = ORIENTED_EDGE ( 'NONE', *, *, #2681, .F. ) ;
#4617 = APPLICATION_CONTEXT ( 'automotive_design' ) ;
#4618 = DIRECTION ( 'NONE',  ( 1.000000000000000000, 0.000000000000000000, -0.000000000000000000 ) ) ;
#4619 = CYLINDRICAL_SURFACE ( 'NONE', #13606, 5.000000000000004441 ) ;
#4620 = ADVANCED_FACE ( 'NONE', ( #13677 ), #5624, .F. ) ;
#4621 = EDGE_CURVE ( 'NONE', #5464, #5020, #3082, .T. ) ;
#4622 = ADVANCED_FACE ( 'NONE', ( #4730 ), #5975, .F. ) ;
#4623 = CARTESIAN_POINT ( 'NONE',  ( -15.00000000000001421, 90.00000000000000000, -13.00000000000000000 ) ) ;
#4624 = CARTESIAN_POINT ( 'NONE',  ( -207.4300157105866447, 174.9998640698394468, 3.994873866052218947 ) ) ;
#4625 = EDGE_CURVE ( 'NONE', #5289, #8027, #9946, .T. ) ;
#4626 = CARTESIAN_POINT ( 'NONE',  ( -7.379000772444995526, 30.00000000000000000, 13.00000000000000178 ) ) ;
#4627 = CARTESIAN_POINT ( 'NONE',  ( -32.43085388486576193, 119.6546501525736375, 5.312352690998810800 ) ) ;
#4628 = DIRECTION ( 'NONE',  ( 0.000000000000000000, 1.000000000000000000, 0.000000000000000000 ) ) ;
#4629 = EDGE_LOOP ( 'NONE', ( #13160, #3123, #3843, #6326 ) ) ;
#4630 = DIRECTION ( 'NONE',  ( -1.000000000000000000, -0.000000000000000000, -0.000000000000000000 ) ) ;
#4631 = ORIENTED_EDGE ( 'NONE', *, *, #12739, .F. ) ;
#4632 = LINE ( 'NONE', #16499, #16937 ) ;
#4633 = DIRECTION ( 'NONE',  ( -0.000000000000000000, -0.000000000000000000, -1.000000000000000000 ) ) ;
#4634 = ORIENTED_EDGE ( 'NONE', *, *, #17098, .T. ) ;
#4635 = CARTESIAN_POINT ( 'NONE',  ( -207.6513770290094669, 172.0602489905835171, 0.7577244044828906899 ) ) ;
#4636 = CARTESIAN_POINT ( 'NONE',  ( 34.93420767782698988, 19.99999999999999645, 6.321724734770472587 ) ) ;
#4637 = CARTESIAN_POINT ( 'NONE',  ( -138.7106781186547266, 171.6227766016838245, -2.602085213965210642E-15 ) ) ;
#4638 = ORIENTED_EDGE ( 'NONE', *, *, #1257, .F. ) ;
#4639 = DIRECTION ( 'NONE',  ( 0.000000000000000000, 0.000000000000000000, 1.000000000000000000 ) ) ;
#4640 = CARTESIAN_POINT ( 'NONE',  ( -82.50000000000001421, 196.6227766016838245, -16.00000000000000000 ) ) ;
#4641 = DIRECTION ( 'NONE',  ( -0.000000000000000000, -0.000000000000000000, 1.000000000000000000 ) ) ;
#4642 = CARTESIAN_POINT ( 'NONE',  ( -27.98221281347037959, 30.00000000000000000, 0.000000000000000000 ) ) ;
#4643 = DIRECTION ( 'NONE',  ( 1.000000000000000000, 0.000000000000000000, 0.000000000000000000 ) ) ;
#4644 = CARTESIAN_POINT ( 'NONE',  ( -8.542481054582452771, 30.38359229753140767, -12.94984885967198451 ) ) ;
#4645 = ORIENTED_EDGE ( 'NONE', *, *, #8937, .F. ) ;
#4646 = CARTESIAN_POINT ( 'NONE',  ( -74.25794599717355027, 198.3976433773785004, -22.54711430683564544 ) ) ;
#4647 = CARTESIAN_POINT ( 'NONE',  ( -50.00000000000000711, -20.00000000000000000, 35.00000000000000711 ) ) ;
#4648 = ORIENTED_EDGE ( 'NONE', *, *, #2590, .T. ) ;
#4649 = CARTESIAN_POINT ( 'NONE',  ( -23.00000000000000000, 120.0000000000000284, 0.000000000000000000 ) ) ;
#4650 = FACE_BOUND ( 'NONE', #13800, .T. ) ;
#4651 = EDGE_LOOP ( 'NONE', ( #2649, #6486, #79, #3402 ) ) ;
#4652 = AXIS2_PLACEMENT_3D ( 'NONE', #17409, #13935, #6610 ) ;
#4653 = ORIENTED_EDGE ( 'NONE', *, *, #10399, .T. ) ;
#4654 = DIRECTION ( 'NONE',  ( -0.000000000000000000, 1.000000000000000000, -0.000000000000000000 ) ) ;
#4655 = ORIENTED_EDGE ( 'NONE', *, *, #17198, .T. ) ;
#4656 = ADVANCED_FACE ( 'NONE', ( #15522 ), #15346, .F. ) ;
#4657 = DIRECTION ( 'NONE',  ( -0.8571673013836867971, 0.000000000000000000, -0.5150380737757237481 ) ) ;
#4658 = ORIENTED_EDGE ( 'NONE', *, *, #7378, .F. ) ;
#4659 = CARTESIAN_POINT ( 'NONE',  ( 23.57895800238926043, 142.7196187763571231, -15.94638436093396727 ) ) ;
#4660 = CARTESIAN_POINT ( 'NONE',  ( 15.56337975240373872, 125.2134999403456135, 4.999999999999997335 ) ) ;
#4661 = CARTESIAN_POINT ( 'NONE',  ( -50.00000000000000000, 171.6227766016838245, 19.49999999999998224 ) ) ;
#4662 = CYLINDRICAL_SURFACE ( 'NONE', #4676, 248.0000000000000000 ) ;
#4663 = CIRCLE ( 'NONE', #17088, 10.00000000000000178 ) ;
#4664 = VERTEX_POINT ( 'NONE', #11365 ) ;
#4665 = CARTESIAN_POINT ( 'NONE',  ( 27.92535256414491585, 142.0696621759509526, 14.68466941333283238 ) ) ;
#4666 = DIRECTION ( 'NONE',  ( -1.000000000000000000, 0.000000000000000000, 0.000000000000000000 ) ) ;
#4667 = FACE_OUTER_BOUND ( 'NONE', #4186, .T. ) ;
#4668 = CARTESIAN_POINT ( 'NONE',  ( -20.86241502029082184, 19.99999999999999645, -20.14618526196967352 ) ) ;
#4669 = DIRECTION ( 'NONE',  ( -0.000000000000000000, -0.000000000000000000, -1.000000000000000000 ) ) ;
#4670 = CIRCLE ( 'NONE', #16831, 27.69059892324149530 ) ;
#4671 = CARTESIAN_POINT ( 'NONE',  ( -68.00000000000000000, 171.6227766016838245, 0.000000000000000000 ) ) ;
#4672 = AXIS2_PLACEMENT_3D ( 'NONE', #5839, #1690, #352 ) ;
#4673 = ORIENTED_EDGE ( 'NONE', *, *, #2680, .T. ) ;
#4674 = ADVANCED_FACE ( 'NONE', ( #12605 ), #5786, .F. ) ;
#4675 = CARTESIAN_POINT ( 'NONE',  ( 27.48361012698968864, 136.6227766016838245, 0.000000000000000000 ) ) ;
#4676 = AXIS2_PLACEMENT_3D ( 'NONE', #9886, #11470, #1749 ) ;
#4677 = ORIENTED_EDGE ( 'NONE', *, *, #9264, .T. ) ;
#4678 =( NAMED_UNIT ( * ) SI_UNIT ( $, .STERADIAN. ) SOLID_ANGLE_UNIT ( ) );
#4679 = CARTESIAN_POINT ( 'NONE',  ( -95.00000000000000000, 171.6227766016838245, 27.69059892324149530 ) ) ;
#4680 = CARTESIAN_POINT ( 'NONE',  ( 48.00000000000000711, 155.6227766016839098, 10.00000337241049309 ) ) ;
#4681 = EDGE_CURVE ( 'NONE', #647, #8265, #12257, .T. ) ;
#4682 = ADVANCED_FACE ( 'NONE', ( #1806 ), #5351, .F. ) ;
#4683 = B_SPLINE_CURVE_WITH_KNOTS ( 'NONE', 3,
 ( #3653, #12778, #14362, #10277, #736, #11358, #4721, #565, #2231, #13040, #1976, #6131, #3304, #11527, #12949, #4809, #6298, #11687, #17099, #10365, #15775, #16768, #10203, #7379, #9043 ),
 .UNSPECIFIED., .F., .F.,
 ( 4, 2, 2, 1, 2, 2, 2, 2, 2, 2, 2, 2, 4 ),
 ( 0.000000000000000000, 0.003937549356687076833, 0.005906324035030613949, 0.007875098713374151932, 0.009843873391717689048, 0.01181264807006122616, 0.01575019742674830733, 0.01771897210509184445, 0.01968774678343538503, 0.02362529614012245927, 0.02559407081846599985, 0.02756284549680953697, 0.03150039485349661467 ),
 .UNSPECIFIED. ) ;
#4684 = CARTESIAN_POINT ( 'NONE',  ( -16.30611068361787019, 32.76923076923078781, -15.00000000000000000 ) ) ;
#4685 = EDGE_CURVE ( 'NONE', #14680, #13439, #11972, .T. ) ;
#4686 = EDGE_LOOP ( 'NONE', ( #6452, #4784, #13062, #15127 ) ) ;
#4687 = CARTESIAN_POINT ( 'NONE',  ( 48.00000000000000711, 183.6227766016837961, -8.071800142134975431 ) ) ;
#4688 = CARTESIAN_POINT ( 'NONE',  ( 1.559999999999998943, 1.299038105676664223, -0.7500000000000006661 ) ) ;
#4689 = VECTOR ( 'NONE', #7580, 1000.000000000000000 ) ;
#4690 = CARTESIAN_POINT ( 'NONE',  ( -84.18228968272714496, 199.3779494270211785, 17.85644994789933904 ) ) ;
#4691 = AXIS2_PLACEMENT_3D ( 'NONE', #12596, #463, #8528 ) ;
#4692 =( NAMED_UNIT ( * ) SI_UNIT ( $, .STERADIAN. ) SOLID_ANGLE_UNIT ( ) );
#4693 = EDGE_LOOP ( 'NONE', ( #13855, #16264, #6802, #17400 ) ) ;
#4694 = ORIENTED_EDGE ( 'NONE', *, *, #2875, .F. ) ;
#4695 = DIRECTION ( 'NONE',  ( -0.000000000000000000, -0.000000000000000000, 1.000000000000000000 ) ) ;
#4696 = CARTESIAN_POINT ( 'NONE',  ( 4.755015822784812052, 0.000000000000000000, 0.000000000000000000 ) ) ;
#4697 = EDGE_LOOP ( 'NONE', ( #848, #12301 ) ) ;
#4698 = CYLINDRICAL_SURFACE ( 'NONE', #1330, 2.500000000000000444 ) ;
#4699 = CARTESIAN_POINT ( 'NONE',  ( 8.904477399773945479, 144.1137579919043787, -18.22932967255391290 ) ) ;
#4700 = AXIS2_PLACEMENT_3D ( 'NONE', #7037, #2701, #11016 ) ;
#4701 = VERTEX_POINT ( 'NONE', #2410 ) ;
#4702 = AXIS2_PLACEMENT_3D ( 'NONE', #10035, #3414, #16785 ) ;
#4703 = LINE ( 'NONE', #10092, #1698 ) ;
#4704 = UNCERTAINTY_MEASURE_WITH_UNIT (LENGTH_MEASURE( 1.000000000000000082E-05 ), #1825, 'distance_accuracy_value', 'NONE');
#4705 = DIRECTION ( 'NONE',  ( 0.000000000000000000, 0.000000000000000000, 1.000000000000000000 ) ) ;
#4706 = DIRECTION ( 'NONE',  ( -0.000000000000000000, -0.000000000000000000, 1.000000000000000000 ) ) ;
#4707 = CARTESIAN_POINT ( 'NONE',  ( -25.81900932159184592, 18.00000000000000000, 13.95463872937486194 ) ) ;
#4708 = CARTESIAN_POINT ( 'NONE',  ( 25.49999999999998579, 9.999999999999998224, 0.000000000000000000 ) ) ;
#4709 = AXIS2_PLACEMENT_3D ( 'NONE', #15230, #11067, #14967 ) ;
#4710 = DIRECTION ( 'NONE',  ( -0.000000000000000000, -0.000000000000000000, -1.000000000000000000 ) ) ;
#4711 = VECTOR ( 'NONE', #9483, 1000.000000000000000 ) ;
#4712 = ORIENTED_EDGE ( 'NONE', *, *, #8388, .T. ) ;
#4713 = CARTESIAN_POINT ( 'NONE',  ( 8.602893093599609742, 142.4623620169580818, -19.35743923737696903 ) ) ;
#4714 = VECTOR ( 'NONE', #2657, 1000.000000000000000 ) ;
#4715 = ORIENTED_EDGE ( 'NONE', *, *, #16713, .F. ) ;
#4716 = LINE ( 'NONE', #6042, #11280 ) ;
#4717 = EDGE_CURVE ( 'NONE', #8095, #6914, #7715, .T. ) ;
#4718 = CARTESIAN_POINT ( 'NONE',  ( -27.94760966554430937, 18.00000000000000355, -6.338314452217974626 ) ) ;
#4719 = EDGE_CURVE ( 'NONE', #5469, #10903, #11843, .T. ) ;
#4720 = VERTEX_POINT ( 'NONE', #6227 ) ;
#4721 = CARTESIAN_POINT ( 'NONE',  ( 22.61491075001043782, 19.99999999999999645, 23.50024419593056635 ) ) ;
#4722 = CARTESIAN_POINT ( 'NONE',  ( 19.93228116232496205, 29.93335004877557282, 13.66730128329526650 ) ) ;
#4723 = DIRECTION ( 'NONE',  ( -1.000000000000000000, -0.000000000000000000, 0.000000000000000000 ) ) ;
#4724 = B_SPLINE_CURVE_WITH_KNOTS ( 'NONE', 3,
 ( #6529, #2274, #17234, #17140, #869, #5109, #13346, #15820, #15991, #3606, #10315, #17054, #4923, #13078, #3695, #2547, #9169, #10238, #1207, #15724, #3876, #16982, #945, #10407, #7581, #2183, #13255, #7669, #6334, #15637, #3515, #9260, #2447, #8903, #11727, #6433, #5016, #6611, #3774, #17320, #9083, #14489 ),
 .UNSPECIFIED., .F., .F.,
 ( 4, 2, 2, 2, 2, 2, 2, 2, 2, 2, 2, 2, 2, 2, 2, 2, 2, 2, 2, 2, 4 ),
 ( 0.000000000000000000, 0.002803867404946438179, 0.004205801107419684590, 0.005607734809892931001, 0.007009668512366177412, 0.008411602214839424690, 0.009112569066076062207, 0.009813535917312697990, 0.01051450276854933551, 0.01086498619416765427, 0.01121546961978597302, 0.01156595304540429005, 0.01191643647102261228, 0.01261740332225922898, 0.01331837017349584741, 0.01401933702473246238, 0.01542127072720567843, 0.01682320442967889448, 0.01822513813215211401, 0.01962707183462532659, 0.02243093923957175523 ),
 .UNSPECIFIED. ) ;
#4725 = EDGE_LOOP ( 'NONE', ( #8914, #2238, #16714, #1120 ) ) ;
#4726 = DIRECTION ( 'NONE',  ( 0.000000000000000000, 0.000000000000000000, 1.000000000000000000 ) ) ;
#4727 = VECTOR ( 'NONE', #265, 1000.000000000000000 ) ;
#4728 = DIRECTION ( 'NONE',  ( -1.000000000000000000, 0.000000000000000000, 0.000000000000000000 ) ) ;
#4729 = VECTOR ( 'NONE', #11399, 1000.000000000000000 ) ;
#4730 = FACE_OUTER_BOUND ( 'NONE', #10993, .T. ) ;
#4731 = CARTESIAN_POINT ( 'NONE',  ( -8.058782516633090864, 30.15486961025272450, -15.00000000000000178 ) ) ;
#4732 = DIRECTION ( 'NONE',  ( 0.000000000000000000, 0.000000000000000000, -1.000000000000000000 ) ) ;
#4733 = DIRECTION ( 'NONE',  ( 1.000000000000000000, 0.000000000000000000, 0.000000000000000000 ) ) ;
#4734 = ORIENTED_EDGE ( 'NONE', *, *, #12950, .F. ) ;
#4735 = CARTESIAN_POINT ( 'NONE',  ( -32.43085388486576903, 100.3453498474263768, 5.312352690998809024 ) ) ;
#4736 = CARTESIAN_POINT ( 'NONE',  ( -153.0000000000000284, 171.6227766016838245, 0.000000000000000000 ) ) ;
#4737 = ORIENTED_EDGE ( 'NONE', *, *, #13973, .F. ) ;
#4738 = DIRECTION ( 'NONE',  ( 0.000000000000000000, 1.000000000000000000, 0.000000000000000000 ) ) ;
#4739 = FACE_BOUND ( 'NONE', #6262, .T. ) ;
#4740 = EDGE_CURVE ( 'NONE', #15841, #13489, #3661, .T. ) ;
#4741 = EDGE_LOOP ( 'NONE', ( #2250, #16892, #13997, #7120 ) ) ;
#4742 = ADVANCED_FACE ( 'NONE', ( #6303 ), #12958, .F. ) ;
#4743 = VECTOR ( 'NONE', #5559, 1000.000000000000000 ) ;
#4744 = EDGE_CURVE ( 'NONE', #3385, #15774, #9293, .T. ) ;
#4745 = ORIENTED_EDGE ( 'NONE', *, *, #13936, .T. ) ;
#4746 = ADVANCED_FACE ( 'NONE', ( #3932 ), #6394, .T. ) ;
#4747 = AXIS2_PLACEMENT_3D ( 'NONE', #15284, #10041, #3420 ) ;
#4748 = VERTEX_POINT ( 'NONE', #13046 ) ;
#4749 = CARTESIAN_POINT ( 'NONE',  ( 27.50000000000001066, 146.6227766016838245, 10.00000000000000178 ) ) ;
#4750 = ORIENTED_EDGE ( 'NONE', *, *, #1574, .F. ) ;
#4751 = CARTESIAN_POINT ( 'NONE',  ( 15.00000000000000000, 171.6227766016838245, 0.000000000000000000 ) ) ;
#4752 = CARTESIAN_POINT ( 'NONE',  ( 8.630636718464335999, 133.1548047818457690, 12.68018750699619268 ) ) ;
#4753 = DIRECTION ( 'NONE',  ( 1.000000000000000000, 0.000000000000000000, 0.000000000000000000 ) ) ;
#4754 = CARTESIAN_POINT ( 'NONE',  ( 13.66341101666136382, 138.6227766017534293, 1.153153160045991887 ) ) ;
#4755 = AXIS2_PLACEMENT_3D ( 'NONE', #8455, #12443, #481 ) ;
#4756 = AXIS2_PLACEMENT_3D ( 'NONE', #12601, #969, #4639 ) ;
#4757 =( GEOMETRIC_REPRESENTATION_CONTEXT ( 3 ) GLOBAL_UNCERTAINTY_ASSIGNED_CONTEXT ( ( #2046 ) ) GLOBAL_UNIT_ASSIGNED_CONTEXT ( ( #7499, #10066, #10160 ) ) REPRESENTATION_CONTEXT ( 'NONE', 'WORKASPACE' ) );
#4758 = VERTEX_POINT ( 'NONE', #915 ) ;
#4759 = CARTESIAN_POINT ( 'NONE',  ( 25.00000000000000711, 146.6227766016838245, 21.54065922853802562 ) ) ;
#4760 = DIRECTION ( 'NONE',  ( 0.000000000000000000, -1.000000000000000000, 6.123233995736762338E-17 ) ) ;
#4761 = CYLINDRICAL_SURFACE ( 'NONE', #15843, 10.00000000000000178 ) ;
#4762 = EDGE_CURVE ( 'NONE', #13399, #14544, #4026, .T. ) ;
#4763 = CARTESIAN_POINT ( 'NONE',  ( -13.98869899561406882, 20.00000000000231637, -10.23150106588177621 ) ) ;
#4764 = CARTESIAN_POINT ( 'NONE',  ( -100.0000000000000000, 100.0000000000000142, 6.000000000000000000 ) ) ;
#4765 = PRODUCT ( 'torque adjustment ring', 'torque adjustment ring', '', ( #10225 ) ) ;
#4766 = LINE ( 'NONE', #10156, #2266 ) ;
#4767 = CIRCLE ( 'NONE', #15220, 19.49999999999998224 ) ;
#4768 = ORIENTED_EDGE ( 'NONE', *, *, #15114, .T. ) ;
#4769 = DIRECTION ( 'NONE',  ( 1.000000000000000000, -0.000000000000000000, -0.000000000000000000 ) ) ;
#4770 = VECTOR ( 'NONE', #6346, 1000.000000000000000 ) ;
#4771 = ORIENTED_EDGE ( 'NONE', *, *, #7430, .T. ) ;
#4772 = SHAPE_REPRESENTATION_RELATIONSHIP ( 'NONE' , 'NONE' ,  #13460, #10572 ) ;
#4773 = LINE ( 'NONE', #2190, #16125 ) ;
#4774 = DIRECTION ( 'NONE',  ( 0.000000000000000000, 0.000000000000000000, 1.000000000000000000 ) ) ;
#4775 = CARTESIAN_POINT ( 'NONE',  ( 196.0000000000000000, 163.6227766016838530, -10.00000337241049309 ) ) ;
#4776 = EDGE_LOOP ( 'NONE', ( #8635, #4095, #9894, #14047 ) ) ;
#4777 = DIRECTION ( 'NONE',  ( 0.000000000000000000, 0.000000000000000000, 1.000000000000000000 ) ) ;
#4778 = CIRCLE ( 'NONE', #5347, 30.00000000000000000 ) ;
#4779 = CARTESIAN_POINT ( 'NONE',  ( -73.00000000000001421, 171.6227766016838245, 0.000000000000000000 ) ) ;
#4780 = AXIS2_PLACEMENT_3D ( 'NONE', #6954, #13422, #9605 ) ;
#4781 = FACE_OUTER_BOUND ( 'NONE', #9942, .T. ) ;
#4782 = ADVANCED_FACE ( 'NONE', ( #12320 ), #5689, .F. ) ;
#4783 = ORIENTED_EDGE ( 'NONE', *, *, #12472, .F. ) ;
#4784 = ORIENTED_EDGE ( 'NONE', *, *, #7869, .F. ) ;
#4785 = CARTESIAN_POINT ( 'NONE',  ( 19.96520957614361436, 19.99999999999885603, -13.72477420846906249 ) ) ;
#4786 = CARTESIAN_POINT ( 'NONE',  ( -100.0000000000000000, 199.3133755249253056, -1.695560166891042033E-15 ) ) ;
#4787 = ORIENTED_EDGE ( 'NONE', *, *, #7866, .F. ) ;
#4788 = EDGE_CURVE ( 'NONE', #13275, #15996, #1521, .T. ) ;
#4789 = DIRECTION ( 'NONE',  ( 1.000000000000000000, 0.000000000000000000, 0.000000000000000000 ) ) ;
#4790 = ADVANCED_FACE ( 'NONE', ( #2933 ), #5431, .F. ) ;
#4791 = CYLINDRICAL_SURFACE ( 'NONE', #10620, 10.00000000000000178 ) ;
#4792 = AXIS2_PLACEMENT_3D ( 'NONE', #8898, #4588, #14306 ) ;
#4793 = ORIENTED_EDGE ( 'NONE', *, *, #8994, .T. ) ;
#4794 = AXIS2_PLACEMENT_3D ( 'NONE', #15862, #11522, #3736 ) ;
#4795 = DIRECTION ( 'NONE',  ( 0.000000000000000000, 0.000000000000000000, 1.000000000000000000 ) ) ;
#4796 = DIRECTION ( 'NONE',  ( 0.000000000000000000, 1.000000000000000000, 0.000000000000000000 ) ) ;
#4797 = DIRECTION ( 'NONE',  ( -1.000000000000000000, 0.000000000000000000, 0.000000000000000000 ) ) ;
#4798 = CARTESIAN_POINT ( 'NONE',  ( -12.73428483635922426, 18.00000000000460787, 6.504128904294631752 ) ) ;
#4799 = CYLINDRICAL_SURFACE ( 'NONE', #4385, 7.500000000000000000 ) ;
#4800 = CARTESIAN_POINT ( 'NONE',  ( 31.99336486990593542, 140.9591509882843070, -16.87514788462641491 ) ) ;
#4801 = VERTEX_POINT ( 'NONE', #16492 ) ;
#4802 = CARTESIAN_POINT ( 'NONE',  ( 196.0000000000000000, 155.6227766016839098, 15.00000337241049486 ) ) ;
#4803 = AXIS2_PLACEMENT_3D ( 'NONE', #16132, #10, #16215 ) ;
#4804 = ORIENTED_EDGE ( 'NONE', *, *, #9391, .F. ) ;
#4805 = FACE_OUTER_BOUND ( 'NONE', #235, .T. ) ;
#4806 = PRODUCT_DEFINITION ( 'UNKNOWN', '', #1633, #16115 ) ;
#4807 = DIRECTION ( 'NONE',  ( -1.000000000000000000, 0.000000000000000000, 0.000000000000000000 ) ) ;
#4808 = VERTEX_POINT ( 'NONE', #1447 ) ;
#4809 = CARTESIAN_POINT ( 'NONE',  ( 31.20890926080315353, 19.99999999999999289, 16.64259892333393154 ) ) ;
#4810 = EDGE_CURVE ( 'NONE', #14615, #8170, #10820, .T. ) ;
#4811 = FACE_OUTER_BOUND ( 'NONE', #15003, .T. ) ;
#4812 = VECTOR ( 'NONE', #12642, 1000.000000000000000 ) ;
#4813 = AXIS2_PLACEMENT_3D ( 'NONE', #12279, #17336, #2645 ) ;
#4814 = VERTEX_POINT ( 'NONE', #12157 ) ;
#4815 = ITEM_DEFINED_TRANSFORMATION ( 'NONE', 'NONE', #11777,  #3583 ) ;
#4816 = CIRCLE ( 'NONE', #17245, 0.2000000000000000944 ) ;
#4817 = CARTESIAN_POINT ( 'NONE',  ( 48.00000000000000711, 167.6227766016838814, -19.42820660268601074 ) ) ;
#4818 = CARTESIAN_POINT ( 'NONE',  ( -75.00000000000001421, 196.3674529106260422, 21.83698684826043390 ) ) ;
#4819 = CARTESIAN_POINT ( 'NONE',  ( -7.379000772444994638, 30.00000000000000000, -15.00000000000000000 ) ) ;
#4820 = EDGE_CURVE ( 'NONE', #15013, #12351, #17394, .T. ) ;
#4821 = DIRECTION ( 'NONE',  ( 0.000000000000000000, 0.000000000000000000, 1.000000000000000000 ) ) ;
#4822 = FACE_OUTER_BOUND ( 'NONE', #8261, .T. ) ;
#4823 = ORIENTED_EDGE ( 'NONE', *, *, #1794, .T. ) ;
#4824 = LINE ( 'NONE', #11701, #17191 ) ;
#4825 = CARTESIAN_POINT ( 'NONE',  ( -27.81025873171733664, 19.99999999999999289, -7.666431193274479305 ) ) ;
#4826 = ORIENTED_EDGE ( 'NONE', *, *, #15766, .F. ) ;
#4827 = CARTESIAN_POINT ( 'NONE',  ( 34.82914105512134029, 193.0398713882428012, -27.68487141596273915 ) ) ;
#4828 = DIRECTION ( 'NONE',  ( -0.000000000000000000, -0.000000000000000000, -1.000000000000000000 ) ) ;
#4829 = AXIS2_PLACEMENT_3D ( 'NONE', #11999, #14921, #8191 ) ;
#4830 = ORIENTED_EDGE ( 'NONE', *, *, #12515, .T. ) ;
#4831 = ORIENTED_EDGE ( 'NONE', *, *, #7115, .F. ) ;
#4832 = ORIENTED_EDGE ( 'NONE', *, *, #1599, .T. ) ;
#4833 = AXIS2_PLACEMENT_3D ( 'NONE', #14393, #17123, #5002 ) ;
#4834 = ORIENTED_EDGE ( 'NONE', *, *, #10792, .F. ) ;
#4835 = CARTESIAN_POINT ( 'NONE',  ( -72.74907522843312790, 148.5867852293671092, -23.63587233142069621 ) ) ;
#4836 = ORIENTED_EDGE ( 'NONE', *, *, #7483, .F. ) ;
#4837 = CARTESIAN_POINT ( 'NONE',  ( 22.78662571002525183, 144.5042670319084266, -18.82352572523457113 ) ) ;
#4838 = DIRECTION ( 'NONE',  ( -0.000000000000000000, -0.000000000000000000, -1.000000000000000000 ) ) ;
#4839 = DIRECTION ( 'NONE',  ( 1.000000000000000000, 0.000000000000000000, 0.000000000000000000 ) ) ;
#4840 = AXIS2_PLACEMENT_3D ( 'NONE', #16608, #8625, #15008 ) ;
#4841 = EDGE_CURVE ( 'NONE', #7936, #2922, #8656, .T. ) ;
#4842 = CARTESIAN_POINT ( 'NONE',  ( 22.73076297281406255, 29.84603606043824442, 6.815711530131156159 ) ) ;
#4843 = EDGE_CURVE ( 'NONE', #978, #13751, #9458, .T. ) ;
#4844 = DIRECTION ( 'NONE',  ( -1.000000000000000000, -0.000000000000000000, -0.000000000000000000 ) ) ;
#4845 = ADVANCED_FACE ( 'NONE', ( #5510 ), #2855, .F. ) ;
#4846 = ORIENTED_EDGE ( 'NONE', *, *, #11525, .F. ) ;
#4847 = DIRECTION ( 'NONE',  ( 0.9961946980917465444, -0.04357787137382451714, 0.07547908730516460218 ) ) ;
#4848 = CARTESIAN_POINT ( 'NONE',  ( -116.4755503550297107, 171.6227766016838245, -78.75916623668499028 ) ) ;
#4849 = CARTESIAN_POINT ( 'NONE',  ( -14.66060021943728486, 20.00000000000115818, -8.782938007015319570 ) ) ;
#4850 = CARTESIAN_POINT ( 'NONE',  ( -74.00000000000001421, 196.6227766016838245, -16.00000000000000000 ) ) ;
#4851 = AXIS2_PLACEMENT_3D ( 'NONE', #1640, #12786, #12698 ) ;
#4852 = CARTESIAN_POINT ( 'NONE',  ( -187.6513770290094669, 172.4976050944027008, -2.196701325097758062 ) ) ;
#4853 = VERTEX_POINT ( 'NONE', #9402 ) ;
#4854 = DIRECTION ( 'NONE',  ( 0.000000000000000000, 0.000000000000000000, -1.000000000000000000 ) ) ;
#4855 = VERTEX_POINT ( 'NONE', #10898 ) ;
#4856 = LINE ( 'NONE', #16731, #5377 ) ;
#4857 = CARTESIAN_POINT ( 'NONE',  ( -147.9615242270661213, 171.6227766016838245, 0.000000000000000000 ) ) ;
#4858 = CARTESIAN_POINT ( 'NONE',  ( 10.21857696054809317, 131.9747203951183110, -12.11181647197579636 ) ) ;
#4859 = EDGE_LOOP ( 'NONE', ( #12124, #5327, #2758, #14191 ) ) ;
#4860 = DIRECTION ( 'NONE',  ( 1.000000000000000000, 6.938893903907228378E-16, 0.000000000000000000 ) ) ;
#4861 = CARTESIAN_POINT ( 'NONE',  ( -725.0000000000000000, 30.00000000000000000, -15.00000000000000000 ) ) ;
#4862 = CARTESIAN_POINT ( 'NONE',  ( 30.00000000000001066, 146.6227766016838245, 10.00000000000000178 ) ) ;
#4863 = CARTESIAN_POINT ( 'NONE',  ( 33.47930603387190018, 201.5149201033276825, -18.20725769141082040 ) ) ;
#4864 = VERTEX_POINT ( 'NONE', #7988 ) ;
#4865 = ORIENTED_EDGE ( 'NONE', *, *, #8845, .F. ) ;
#4866 = CARTESIAN_POINT ( 'NONE',  ( 20.25331481973466907, 19.99999999999999289, -13.55662431013403868 ) ) ;
#4867 = CARTESIAN_POINT ( 'NONE',  ( -725.0000000000000000, 19.99999999999995737, 15.00000000000000000 ) ) ;
#4868 = EDGE_LOOP ( 'NONE', ( #11683, #4281 ) ) ;
#4869 = DIRECTION ( 'NONE',  ( 0.000000000000000000, 0.000000000000000000, -1.000000000000000000 ) ) ;
#4870 = CARTESIAN_POINT ( 'NONE',  ( 39.99999999999998579, -20.00000000000000000, -35.00000000000002132 ) ) ;
#4871 = VERTEX_POINT ( 'NONE', #4355 ) ;
#4872 = FACE_OUTER_BOUND ( 'NONE', #16479, .T. ) ;
#4873 = ADVANCED_FACE ( 'NONE', ( #16320 ), #13656, .T. ) ;
#4874 = CARTESIAN_POINT ( 'NONE',  ( 48.00000000000000711, 155.6227766016839098, -12.50000337241049309 ) ) ;
#4875 = ADVANCED_BREP_SHAPE_REPRESENTATION ( '', ( #16934, #3583 ), #14620 ) ;
#4876 = CARTESIAN_POINT ( 'NONE',  ( -725.0000000000000000, 19.99999999999995737, 4.999999999999997335 ) ) ;
#4877 = CARTESIAN_POINT ( 'NONE',  ( -14.94236098988382722, 32.37030496448370798, 9.276599271047366813 ) ) ;
#4878 = FACE_OUTER_BOUND ( 'NONE', #292, .T. ) ;
#4879 = CARTESIAN_POINT ( 'NONE',  ( 36.00000000000002132, 145.8714137932802828, -23.72804097270956447 ) ) ;
#4880 = ORIENTED_EDGE ( 'NONE', *, *, #2145, .T. ) ;
#4881 = LINE ( 'NONE', #4802, #14940 ) ;
#4882 = VERTEX_POINT ( 'NONE', #9744 ) ;
#4883 = DIRECTION ( 'NONE',  ( 0.000000000000000000, 0.000000000000000000, -1.000000000000000000 ) ) ;
#4884 = DIRECTION ( 'NONE',  ( -0.000000000000000000, -0.000000000000000000, -1.000000000000000000 ) ) ;
#4885 = ORIENTED_EDGE ( 'NONE', *, *, #3635, .F. ) ;
#4886 = DIRECTION ( 'NONE',  ( 1.000000000000000000, 0.000000000000000000, 0.000000000000000000 ) ) ;
#4887 = CARTESIAN_POINT ( 'NONE',  ( 24.99836435517920918, 19.99999999999999289, 6.327826241642252825 ) ) ;
#4888 = EDGE_CURVE ( 'NONE', #7725, #17193, #10115, .T. ) ;
#4889 = EDGE_LOOP ( 'NONE', ( #11611, #4010 ) ) ;
#4890 = DIRECTION ( 'NONE',  ( 0.000000000000000000, -0.5000000000000011102, 0.8660254037844380415 ) ) ;
#4891 = DIRECTION ( 'NONE',  ( 1.000000000000000000, 0.000000000000000000, -0.000000000000000000 ) ) ;
#4892 = ADVANCED_FACE ( 'NONE', ( #3114 ), #14187, .T. ) ;
#4893 = DIRECTION ( 'NONE',  ( -1.000000000000000000, -0.000000000000000000, 0.000000000000000000 ) ) ;
#4894 = CARTESIAN_POINT ( 'NONE',  ( -24.81085081034726869, 18.00000000000000000, -15.69149817755460496 ) ) ;
#4895 = EDGE_CURVE ( 'NONE', #12240, #8170, #6031, .T. ) ;
#4896 = ADVANCED_FACE ( 'NONE', ( #5768 ), #15411, .T. ) ;
#4897 = EDGE_LOOP ( 'NONE', ( #7562, #7940 ) ) ;
#4898 = LINE ( 'NONE', #11887, #8985 ) ;
#4899 = CARTESIAN_POINT ( 'NONE',  ( -11.98734322101357641, 20.00000000000000000, -24.50584837321703802 ) ) ;
#4900 = ORIENTED_EDGE ( 'NONE', *, *, #144, .T. ) ;
#4901 = CARTESIAN_POINT ( 'NONE',  ( 30.91081357902854521, 190.6879887351488776, -29.35163774059939712 ) ) ;
#4902 = DIRECTION ( 'NONE',  ( 0.000000000000000000, -1.000000000000000000, 8.673617379884035472E-16 ) ) ;
#4903 = EDGE_LOOP ( 'NONE', ( #1660, #1394, #9400, #7819, #14356, #15989 ) ) ;
#4904 = ORIENTED_EDGE ( 'NONE', *, *, #13206, .F. ) ;
#4905 = ORIENTED_EDGE ( 'NONE', *, *, #17266, .T. ) ;
#4906 = ADVANCED_FACE ( 'NONE', ( #11253 ), #8891, .T. ) ;
#4907 = CARTESIAN_POINT ( 'NONE',  ( -72.50000000000002842, 146.9976486552383506, -21.97573418327509742 ) ) ;
#4908 = VERTEX_POINT ( 'NONE', #16576 ) ;
#4909 = SHAPE_REPRESENTATION_RELATIONSHIP ( 'NONE' , 'NONE' ,  #6585, #4875 ) ;
#4910 = LINE ( 'NONE', #14652, #3981 ) ;
#4911 = CARTESIAN_POINT ( 'NONE',  ( -40.00000000000000000, 4.000000000000000000, -30.00000000000000711 ) ) ;
#4912 = CARTESIAN_POINT ( 'NONE',  ( 35.04302060506833527, 149.8947795965756598, -27.44208088385415678 ) ) ;
#4913 = FACE_OUTER_BOUND ( 'NONE', #12663, .T. ) ;
#4914 = CARTESIAN_POINT ( 'NONE',  ( -153.0000000000000284, 171.6227766016838245, 6.000000000000005329 ) ) ;
#4915 = AXIS2_PLACEMENT_3D ( 'NONE', #11281, #4733, #8802 ) ;
#4916 = ORIENTED_EDGE ( 'NONE', *, *, #5599, .T. ) ;
#4917 = CYLINDRICAL_SURFACE ( 'NONE', #17179, 2.500000000000002220 ) ;
#4918 = DIRECTION ( 'NONE',  ( -1.000000000000000000, -0.000000000000000000, -0.000000000000000000 ) ) ;
#4919 = LINE ( 'NONE', #17133, #6517 ) ;
#4920 = CARTESIAN_POINT ( 'NONE',  ( 19.94005785806629660, 29.93324777864367192, 13.66280195656096907 ) ) ;
#4921 = ORIENTED_EDGE ( 'NONE', *, *, #10708, .T. ) ;
#4922 = LINE ( 'NONE', #7489, #4689 ) ;
#4923 = CARTESIAN_POINT ( 'NONE',  ( 27.91212228340977930, 201.1698135001049650, 14.69689982759755154 ) ) ;
#4924 = EDGE_CURVE ( 'NONE', #8768, #8531, #1837, .T. ) ;
#4925 = EDGE_CURVE ( 'NONE', #2195, #554, #10302, .T. ) ;
#4926 = EDGE_CURVE ( 'NONE', #14446, #17286, #16671, .T. ) ;
#4927 = ORIENTED_EDGE ( 'NONE', *, *, #12092, .F. ) ;
#4928 = LINE ( 'NONE', #17324, #14686 ) ;
#4929 = AXIS2_PLACEMENT_3D ( 'NONE', #14613, #7883, #13292 ) ;
#4930 = VERTEX_POINT ( 'NONE', #15242 ) ;
#4931 = LINE ( 'NONE', #14765, #2256 ) ;
#4932 = VECTOR ( 'NONE', #10398, 1000.000000000000000 ) ;
#4933 = DIRECTION ( 'NONE',  ( -0.000000000000000000, -0.000000000000000000, -1.000000000000000000 ) ) ;
#4934 = CARTESIAN_POINT ( 'NONE',  ( -45.00000000000000000, 140.0000000000000000, 0.000000000000000000 ) ) ;
#4935 = CARTESIAN_POINT ( 'NONE',  ( 196.0000000000000000, 175.6227766016838245, 5.571800142134975431 ) ) ;
#4936 = ORIENTED_EDGE ( 'NONE', *, *, #10276, .F. ) ;
#4937 = DIRECTION ( 'NONE',  ( 1.000000000000000000, 0.000000000000000000, 0.000000000000000000 ) ) ;
#4938 = DIRECTION ( 'NONE',  ( 1.000000000000000000, 0.000000000000000000, 0.000000000000000000 ) ) ;
#4939 = APPLICATION_CONTEXT ( 'automotive_design' ) ;
#4940 = CARTESIAN_POINT ( 'NONE',  ( 30.00000000000001066, 146.6227766016838245, 0.000000000000000000 ) ) ;
#4941 = AXIS2_PLACEMENT_3D ( 'NONE', #2048, #4706, #7441 ) ;
#4942 = EDGE_LOOP ( 'NONE', ( #15594, #14816, #10409, #11286, #225, #12496 ) ) ;
#4943 = MECHANICAL_DESIGN_GEOMETRIC_PRESENTATION_REPRESENTATION (  '', ( #3829 ), #16558 ) ;
#4944 = ORIENTED_EDGE ( 'NONE', *, *, #2354, .F. ) ;
#4945 = CARTESIAN_POINT ( 'NONE',  ( 21.54097706593338302, 29.91227807600463606, -12.53500607440986236 ) ) ;
#4946 = CARTESIAN_POINT ( 'NONE',  ( 13.53786153804125725, 141.8544345782132439, -18.40805394434863018 ) ) ;
#4947 = EDGE_CURVE ( 'NONE', #6224, #13521, #11716, .T. ) ;
#4948 = ADVANCED_FACE ( 'NONE', ( #15142, #8516 ), #7271, .T. ) ;
#4949 = EDGE_LOOP ( 'NONE', ( #8589, #3192, #17048, #757 ) ) ;
#4950 = CARTESIAN_POINT ( 'NONE',  ( 27.30499999999999616, 0.000000000000000000, 2.499999999999999556 ) ) ;
#4951 = CARTESIAN_POINT ( 'NONE',  ( 14.50951369217283826, 138.6207054667691523, -6.378636156063609342 ) ) ;
#4952 = ORIENTED_EDGE ( 'NONE', *, *, #790, .T. ) ;
#4953 = CARTESIAN_POINT ( 'NONE',  ( -25.49999999999998579, 10.00000000000000000, -16.00000000000000000 ) ) ;
#4954 =( GEOMETRIC_REPRESENTATION_CONTEXT ( 3 ) GLOBAL_UNCERTAINTY_ASSIGNED_CONTEXT ( ( #3852 ) ) GLOBAL_UNIT_ASSIGNED_CONTEXT ( ( #3163, #14057, #9884 ) ) REPRESENTATION_CONTEXT ( 'NONE', 'WORKASPACE' ) );
#4955 = AXIS2_PLACEMENT_3D ( 'NONE', #17451, #9299, #4009 ) ;
#4956 = CIRCLE ( 'NONE', #5808, 2.500000000000002220 ) ;
#4957 = DIRECTION ( 'NONE',  ( -0.000000000000000000, -0.000000000000000000, -1.000000000000000000 ) ) ;
#4958 = CARTESIAN_POINT ( 'NONE',  ( 34.99999999999999289, 8.000000000000000000, 34.99999999999999289 ) ) ;
#4959 = CARTESIAN_POINT ( 'NONE',  ( -12.51506868919167026, 17.99999999999883826, 7.695309128566540480 ) ) ;
#4960 = CARTESIAN_POINT ( 'NONE',  ( -19.68629150101526903, 125.3137084989847807, 12.99999999999998401 ) ) ;
#4961 = CARTESIAN_POINT ( 'NONE',  ( 35.49675130541458401, 144.1922489206527302, -21.74472059540656943 ) ) ;
#4962 = ORIENTED_EDGE ( 'NONE', *, *, #14013, .F. ) ;
#4963 = FACE_OUTER_BOUND ( 'NONE', #11374, .T. ) ;
#4964 = ORIENTED_EDGE ( 'NONE', *, *, #5442, .F. ) ;
#4965 = EDGE_CURVE ( 'NONE', #2336, #8681, #13924, .T. ) ;
#4966 = CARTESIAN_POINT ( 'NONE',  ( 14.93242934743711992, 30.00000000000000000, -15.00000000000000000 ) ) ;
#4967 = AXIS2_PLACEMENT_3D ( 'NONE', #15434, #7200, #8797 ) ;
#4968 = CARTESIAN_POINT ( 'NONE',  ( -14.54670497998689171, 17.99999999999999645, -23.76610458325318831 ) ) ;
#4969 = CIRCLE ( 'NONE', #12609, 4.750000000000000000 ) ;
#4970 = ORIENTED_EDGE ( 'NONE', *, *, #11200, .T. ) ;
#4971 = DIRECTION ( 'NONE',  ( -1.000000000000000000, 1.040834085586084059E-15, 0.000000000000000000 ) ) ;
#4972 = CARTESIAN_POINT ( 'NONE',  ( -71.66708739526794147, 110.0000000000000142, 4.500000000000000000 ) ) ;
#4973 = VECTOR ( 'NONE', #13632, 1000.000000000000000 ) ;
#4974 = CARTESIAN_POINT ( 'NONE',  ( 24.67949051125555826, 29.87169671703155771, 7.269639412668861489 ) ) ;
#4975 = ORIENTED_EDGE ( 'NONE', *, *, #13167, .T. ) ;
#4976 = PLANE ( 'NONE',  #14587 ) ;
#4977 = TOROIDAL_SURFACE ( 'NONE', #9498, -78.75916623668499028, 110.0000000000000142 ) ;
#4978 = VECTOR ( 'NONE', #12059, 1000.000000000000000 ) ;
#4979 = CARTESIAN_POINT ( 'NONE',  ( 22.50000000000000000, 196.6227766016838245, -21.54065922853802562 ) ) ;
#4980 = CARTESIAN_POINT ( 'NONE',  ( 40.00000000000000711, 196.6227766016838245, 0.000000000000000000 ) ) ;
#4981 = VECTOR ( 'NONE', #3032, 1000.000000000000000 ) ;
#4982 = CARTESIAN_POINT ( 'NONE',  ( -11.84409501751983207, 18.00000000000232703, -9.388895791866135099 ) ) ;
#4983 = ORIENTED_EDGE ( 'NONE', *, *, #7249, .T. ) ;
#4984 = DIRECTION ( 'NONE',  ( -1.156482317317868274E-16, 1.000000000000000000, 0.000000000000000000 ) ) ;
#4985 = EDGE_LOOP ( 'NONE', ( #9864, #1940, #9850 ) ) ;
#4986 = EDGE_CURVE ( 'NONE', #10807, #11033, #11152, .T. ) ;
#4987 = CARTESIAN_POINT ( 'NONE',  ( 196.0000000000000000, 175.6227766016838245, -5.571800142134975431 ) ) ;
#4988 = CARTESIAN_POINT ( 'NONE',  ( 39.99999999999998579, 8.000000000000000000, -29.99999999999999645 ) ) ;
#4989 = VERTEX_POINT ( 'NONE', #10096 ) ;
#4990 = VERTEX_POINT ( 'NONE', #16834 ) ;
#4991 = ORIENTED_EDGE ( 'NONE', *, *, #2990, .T. ) ;
#4992 = VECTOR ( 'NONE', #8844, 1000.000000000000000 ) ;
#4993 = VECTOR ( 'NONE', #11858, 1000.000000000000000 ) ;
#4994 = ADVANCED_FACE ( 'NONE', ( #12676 ), #3381, .F. ) ;
#4995 = AXIS2_PLACEMENT_3D ( 'NONE', #5144, #12787, #4732 ) ;
#4996 = ADVANCED_FACE ( 'NONE', ( #11347, #7365 ), #1707, .F. ) ;
#4997 = CARTESIAN_POINT ( 'NONE',  ( -84.24679270737827608, 152.8105824767975491, -27.11332964807919410 ) ) ;
#4998 = ADVANCED_FACE ( 'NONE', ( #3729 ), #11603, .F. ) ;
#4999 = CIRCLE ( 'NONE', #10074, 4.750000000000000000 ) ;
#5000 = EDGE_LOOP ( 'NONE', ( #17114, #13613, #15672, #16771, #15755, #7909, #14019 ) ) ;
#5001 = DIRECTION ( 'NONE',  ( 0.000000000000000000, 0.000000000000000000, 1.000000000000000000 ) ) ;
#5002 = DIRECTION ( 'NONE',  ( -1.000000000000000000, 0.000000000000000000, 0.000000000000000000 ) ) ;
#5003 = DIRECTION ( 'NONE',  ( 0.000000000000000000, 1.000000000000000000, 0.000000000000000000 ) ) ;
#5004 = CARTESIAN_POINT ( 'NONE',  ( 25.96989122963463004, 151.0873486859325112, -28.34424093584478399 ) ) ;
#5005 = CARTESIAN_POINT ( 'NONE',  ( 22.66736643345232949, 29.84725565559530480, 7.069278529401977984 ) ) ;
#5006 = CARTESIAN_POINT ( 'NONE',  ( -85.00000000000000000, 147.1386660375792417, 22.13939837391654208 ) ) ;
#5007 = VERTEX_POINT ( 'NONE', #17269 ) ;
#5008 = DIRECTION ( 'NONE',  ( -0.000000000000000000, -0.000000000000000000, -1.000000000000000000 ) ) ;
#5009 = LINE ( 'NONE', #17132, #2113 ) ;
#5010 = VECTOR ( 'NONE', #12391, 1000.000000000000000 ) ;
#5011 = DIRECTION ( 'NONE',  ( -1.000000000000000000, 0.000000000000000000, 0.000000000000000000 ) ) ;
#5012 = CARTESIAN_POINT ( 'NONE',  ( 18.16062352778163813, 29.95676120085481386, 14.47054584901207619 ) ) ;
#5013 = ORIENTED_EDGE ( 'NONE', *, *, #15921, .T. ) ;
#5014 = CIRCLE ( 'NONE', #14910, 33.00000000000000000 ) ;
#5015 = EDGE_CURVE ( 'NONE', #11548, #11927, #10874, .T. ) ;
#5016 = CARTESIAN_POINT ( 'NONE',  ( 34.17818013757652551, 199.3841150854655382, 17.84683500849086712 ) ) ;
#5017 = VERTEX_POINT ( 'NONE', #2217 ) ;
#5018 = CARTESIAN_POINT ( 'NONE',  ( -31.89848094669885725, 100.0271397714182342, -5.500000000000000000 ) ) ;
#5019 = FACE_OUTER_BOUND ( 'NONE', #8020, .T. ) ;
#5020 = VERTEX_POINT ( 'NONE', #12936 ) ;
#5021 = AXIS2_PLACEMENT_3D ( 'NONE', #333, #3345, #14148 ) ;
#5022 = DIRECTION ( 'NONE',  ( 0.9961946980917461003, -0.04357787137382628656, 0.07547908730516766918 ) ) ;
#5023 = CONICAL_SURFACE ( 'NONE', #13799, 2.499999999999998668, 1.029744260000002187 ) ;
#5024 = DIRECTION ( 'NONE',  ( 1.000000000000000000, 0.000000000000000000, 0.000000000000000000 ) ) ;
#5025 = CARTESIAN_POINT ( 'NONE',  ( -15.00000000000001421, 90.00000000000000000, 13.00000000000000000 ) ) ;
#5026 = CARTESIAN_POINT ( 'NONE',  ( 11.61330907248435018, 130.6704317944142986, -11.35602788888950698 ) ) ;
#5027 = EDGE_LOOP ( 'NONE', ( #2867, #17235 ) ) ;
#5028 = CARTESIAN_POINT ( 'NONE',  ( -102.0000000000000142, 171.6227766016838245, 0.000000000000000000 ) ) ;
#5029 = CARTESIAN_POINT ( 'NONE',  ( -206.3689767832464668, 173.6103877383153531, -4.531616471133038004 ) ) ;
#5030 = EDGE_CURVE ( 'NONE', #4908, #4748, #984, .T. ) ;
#5031 = CARTESIAN_POINT ( 'NONE',  ( -27.99999999999998224, 10.00000000000000000, -30.00000000000000355 ) ) ;
#5032 = SURFACE_STYLE_USAGE ( .BOTH. , #15836 ) ;
#5033 = EDGE_LOOP ( 'NONE', ( #10481, #12932 ) ) ;
#5034 = VECTOR ( 'NONE', #997, 1000.000000000000000 ) ;
#5035 = VERTEX_POINT ( 'NONE', #10265 ) ;
#5036 = AXIS2_PLACEMENT_3D ( 'NONE', #10966, #15215, #16384 ) ;
#5037 = ORIENTED_EDGE ( 'NONE', *, *, #2622, .T. ) ;
#5038 = CARTESIAN_POINT ( 'NONE',  ( 16.61152767523946139, 141.2200844281568379, -17.35152312112458972 ) ) ;
#5039 = ORIENTED_EDGE ( 'NONE', *, *, #10242, .F. ) ;
#5040 = DIRECTION ( 'NONE',  ( 0.000000000000000000, 0.000000000000000000, 1.000000000000000000 ) ) ;
#5041 = CARTESIAN_POINT ( 'NONE',  ( 10.03770976535549586, 140.0890479961802839, -11.85997561143352996 ) ) ;
#5042 = ORIENTED_EDGE ( 'NONE', *, *, #12324, .F. ) ;
#5043 = DIRECTION ( 'NONE',  ( -1.156482317317868274E-16, 1.000000000000000000, 0.000000000000000000 ) ) ;
#5044 = CARTESIAN_POINT ( 'NONE',  ( -15.00000000000002665, 130.0000000000000000, 15.00000000000000000 ) ) ;
#5045 = CARTESIAN_POINT ( 'NONE',  ( 30.00000000000001066, 146.6227766016838245, 0.000000000000000000 ) ) ;
#5046 = CIRCLE ( 'NONE', #13822, 2.500000000000000000 ) ;
#5047 = CARTESIAN_POINT ( 'NONE',  ( -96.00000000000001421, 171.6227766016838245, 30.00000000000000000 ) ) ;
#5048 = DIRECTION ( 'NONE',  ( 0.000000000000000000, -1.000000000000000000, 0.000000000000000000 ) ) ;
#5049 = DIRECTION ( 'NONE',  ( -1.000000000000000000, -0.000000000000000000, -0.000000000000000000 ) ) ;
#5050 = CARTESIAN_POINT ( 'NONE',  ( -9.925381735234770630, 18.00000000000231992, 11.63955885304398130 ) ) ;
#5051 = EDGE_CURVE ( 'NONE', #11003, #13316, #7698, .T. ) ;
#5052 = EDGE_CURVE ( 'NONE', #3299, #7814, #14838, .T. ) ;
#5053 = FACE_OUTER_BOUND ( 'NONE', #358, .T. ) ;
#5054 = EDGE_CURVE ( 'NONE', #2062, #6313, #2388, .T. ) ;
#5055 = DIRECTION ( 'NONE',  ( -1.000000000000000000, 0.000000000000000000, -5.782411586589356653E-16 ) ) ;
#5056 = EDGE_LOOP ( 'NONE', ( #6270, #2037 ) ) ;
#5057 = DIRECTION ( 'NONE',  ( 0.000000000000000000, 0.000000000000000000, -1.000000000000000000 ) ) ;
#5058 = ORIENTED_EDGE ( 'NONE', *, *, #12886, .F. ) ;
#5059 = DIRECTION ( 'NONE',  ( -1.000000000000000000, 0.000000000000000000, 0.000000000000000000 ) ) ;
#5060 = AXIS2_PLACEMENT_3D ( 'NONE', #12138, #6829, #9 ) ;
#5061 = CARTESIAN_POINT ( 'NONE',  ( -16.40540729975244716, 18.00000000000000000, -23.03124090058167184 ) ) ;
#5062 = VECTOR ( 'NONE', #10747, 1000.000000000000000 ) ;
#5063 = ORIENTED_EDGE ( 'NONE', *, *, #4402, .F. ) ;
#5064 = CARTESIAN_POINT ( 'NONE',  ( -20.86241502029082184, 19.99999999999999645, 20.14618526196967352 ) ) ;
#5065 = CIRCLE ( 'NONE', #1109, 2.499999999999998668 ) ;
#5066 = CARTESIAN_POINT ( 'NONE',  ( 27.25143353317894324, 139.0964629073462220, 5.659441210211040740 ) ) ;
#5067 = CARTESIAN_POINT ( 'NONE',  ( 18.16394926501914497, 19.99999999999886313, 14.51477632729204537 ) ) ;
#5068 = ORIENTED_EDGE ( 'NONE', *, *, #15325, .F. ) ;
#5069 = FACE_OUTER_BOUND ( 'NONE', #681, .T. ) ;
#5070 = CARTESIAN_POINT ( 'NONE',  ( 23.19385591260824597, 193.4380998888852901, -24.76648413410753591 ) ) ;
#5071 = CIRCLE ( 'NONE', #10164, 7.500000000000000000 ) ;
#5072 = CARTESIAN_POINT ( 'NONE',  ( -80.00000000000002842, 146.6227766016838245, 0.000000000000000000 ) ) ;
#5073 = CARTESIAN_POINT ( 'NONE',  ( -12.78422937319141184, 31.72181100014091726, -11.38907491820491913 ) ) ;
#5074 = CIRCLE ( 'NONE', #14971, 5.000000000000004441 ) ;
#5075 = VERTEX_POINT ( 'NONE', #6560 ) ;
#5076 = DIRECTION ( 'NONE',  ( -0.000000000000000000, -0.000000000000000000, 1.000000000000000000 ) ) ;
#5077 = ORIENTED_EDGE ( 'NONE', *, *, #9244, .T. ) ;
#5078 = DIRECTION ( 'NONE',  ( -1.000000000000000000, -0.000000000000000000, 0.000000000000000000 ) ) ;
#5079 = CARTESIAN_POINT ( 'NONE',  ( 49.99999999999998579, 167.6227766016838530, -3.071800142134975431 ) ) ;
#5080 = ORIENTED_EDGE ( 'NONE', *, *, #4257, .F. ) ;
#5081 = ORIENTED_EDGE ( 'NONE', *, *, #3757, .T. ) ;
#5082 = ORIENTED_EDGE ( 'NONE', *, *, #12575, .T. ) ;
#5083 = AXIS2_PLACEMENT_3D ( 'NONE', #16709, #5724, #7628 ) ;
#5084 = AXIS2_PLACEMENT_3D ( 'NONE', #16995, #3712, #9096 ) ;
#5085 = DIRECTION ( 'NONE',  ( -1.000000000000000000, -0.000000000000000000, -0.000000000000000000 ) ) ;
#5086 = UNCERTAINTY_MEASURE_WITH_UNIT (LENGTH_MEASURE( 1.000000000000000082E-05 ), #16360, 'distance_accuracy_value', 'NONE');
#5087 = VECTOR ( 'NONE', #17327, 1000.000000000000000 ) ;
#5088 = ORIENTED_EDGE ( 'NONE', *, *, #114, .T. ) ;
#5089 = DIRECTION ( 'NONE',  ( -1.000000000000000000, 0.000000000000000000, 0.000000000000000000 ) ) ;
#5090 = ADVANCED_FACE ( 'NONE', ( #6467 ), #3254, .T. ) ;
#5091 = DIRECTION ( 'NONE',  ( -1.000000000000000000, 0.000000000000000000, 0.000000000000000000 ) ) ;
#5092 = EDGE_CURVE ( 'NONE', #12797, #1219, #10447, .T. ) ;
#5093 = FILL_AREA_STYLE ('',( #5264 ) ) ;
#5094 = CARTESIAN_POINT ( 'NONE',  ( 35.90034259984014398, 147.9183216992699386, -25.76577836882855266 ) ) ;
#5095 = CARTESIAN_POINT ( 'NONE',  ( 21.87797949700605926, 29.86248177612424115, 9.008363892349379398 ) ) ;
#5096 = CARTESIAN_POINT ( 'NONE',  ( 15.60228996707308191, 124.9392590765123998, 1.671679228207827439 ) ) ;
#5097 = VERTEX_POINT ( 'NONE', #3549 ) ;
#5098 = CARTESIAN_POINT ( 'NONE',  ( 27.42718951882975631, 138.9142741377072525, 4.446260193316556197 ) ) ;
#5099 = AXIS2_PLACEMENT_3D ( 'NONE', #3741, #14531, #189 ) ;
#5100 = AXIS2_PLACEMENT_3D ( 'NONE', #6256, #12898, #8823 ) ;
#5101 = CARTESIAN_POINT ( 'NONE',  ( 22.87571619445694182, 29.89494019521412582, -11.08657135066705379 ) ) ;
#5102 = CARTESIAN_POINT ( 'NONE',  ( 30.49999999999998224, 9.999999999999998224, 1.387778780781445676E-14 ) ) ;
#5103 = FACE_OUTER_BOUND ( 'NONE', #3561, .T. ) ;
#5104 = CIRCLE ( 'NONE', #6225, 2.500000000000002220 ) ;
#5105 = CARTESIAN_POINT ( 'NONE',  ( -18.25212770525992667, 32.30769230769230660, -4.999999999999998224 ) ) ;
#5106 = ORIENTED_EDGE ( 'NONE', *, *, #15224, .T. ) ;
#5107 = LINE ( 'NONE', #10581, #6098 ) ;
#5108 = EDGE_CURVE ( 'NONE', #13611, #8508, #7764, .T. ) ;
#5109 = CARTESIAN_POINT ( 'NONE',  ( 25.81771031727288346, 199.3779494270211785, 17.85644994789938167 ) ) ;
#5110 = EDGE_LOOP ( 'NONE', ( #16478, #16227 ) ) ;
#5111 = DIRECTION ( 'NONE',  ( -1.000000000000000000, -0.000000000000000000, -0.000000000000000000 ) ) ;
#5112 = LINE ( 'NONE', #7750, #13569 ) ;
#5113 = CIRCLE ( 'NONE', #6533, 21.61734737250326077 ) ;
#5114 = ORIENTED_EDGE ( 'NONE', *, *, #2989, .F. ) ;
#5115 = FILL_AREA_STYLE_COLOUR ( '', #11215 ) ;
#5116 = CARTESIAN_POINT ( 'NONE',  ( -77.93691419132714771, 142.0644190903623212, 14.67410160148079967 ) ) ;
#5117 = CARTESIAN_POINT ( 'NONE',  ( 25.49999999999998579, 9.999999999999998224, 10.00000000000000178 ) ) ;
#5118 = CARTESIAN_POINT ( 'NONE',  ( 0.000000000000000000, 1.732050807568885631, 0.000000000000000000 ) ) ;
#5119 = FACE_OUTER_BOUND ( 'NONE', #5307, .T. ) ;
#5120 = PRODUCT_DEFINITION ( 'UNKNOWN', '', #12096, #9369 ) ;
#5121 = VERTEX_POINT ( 'NONE', #3641 ) ;
#5122 = CARTESIAN_POINT ( 'NONE',  ( 39.99999999999997868, 8.000000000000010658, 40.00000000000000711 ) ) ;
#5123 = EDGE_CURVE ( 'NONE', #10007, #8974, #2403, .T. ) ;
#5124 = CARTESIAN_POINT ( 'NONE',  ( -207.2426727481553996, 173.4675081614032877, -4.805322917016542128 ) ) ;
#5125 = CARTESIAN_POINT ( 'NONE',  ( 27.99999999999997513, 4.000000000000000000, -30.00000000000000711 ) ) ;
#5126 = EDGE_CURVE ( 'NONE', #17364, #16020, #16555, .T. ) ;
#5127 = DIRECTION ( 'NONE',  ( 0.000000000000000000, 0.000000000000000000, -1.000000000000000000 ) ) ;
#5128 = EDGE_CURVE ( 'NONE', #9979, #11801, #4670, .T. ) ;
#5129 = CIRCLE ( 'NONE', #16726, 20.00000000000000355 ) ;
#5130 = ORIENTED_EDGE ( 'NONE', *, *, #2938, .F. ) ;
#5131 = VERTEX_POINT ( 'NONE', #8852 ) ;
#5132 = CARTESIAN_POINT ( 'NONE',  ( 6.134011831684059501, 134.2062027339443944, -14.99999999999999822 ) ) ;
#5133 = ORIENTED_EDGE ( 'NONE', *, *, #7920, .F. ) ;
#5134 = LINE ( 'NONE', #7690, #16326 ) ;
#5135 = CARTESIAN_POINT ( 'NONE',  ( 8.856485326996372365, 132.9846638168478137, -12.59946789408625456 ) ) ;
#5136 = ORIENTED_EDGE ( 'NONE', *, *, #13166, .F. ) ;
#5137 = EDGE_CURVE ( 'NONE', #6998, #13633, #15759, .T. ) ;
#5138 = DIRECTION ( 'NONE',  ( -1.000000000000000000, 0.000000000000000000, 0.000000000000000000 ) ) ;
#5139 = DIRECTION ( 'NONE',  ( 1.000000000000000000, 0.000000000000000000, 0.000000000000000000 ) ) ;
#5140 = DIRECTION ( 'NONE',  ( 0.000000000000000000, 1.000000000000000000, 0.000000000000000000 ) ) ;
#5141 = CARTESIAN_POINT ( 'NONE',  ( 32.87600950244731735, 192.5178712342568019, 25.54362227291153786 ) ) ;
#5142 = LINE ( 'NONE', #11512, #4438 ) ;
#5143 = CARTESIAN_POINT ( 'NONE',  ( 34.93420767782698988, 18.00000000000000000, -6.321724734778991106 ) ) ;
#5144 = CARTESIAN_POINT ( 'NONE',  ( 1.559999999999998943, -1.732050807568885631, 0.000000000000000000 ) ) ;
#5145 = DIRECTION ( 'NONE',  ( 0.000000000000000000, 0.000000000000000000, 1.000000000000000000 ) ) ;
#5146 = DIRECTION ( 'NONE',  ( 1.000000000000000000, -0.000000000000000000, -0.000000000000000000 ) ) ;
#5147 = ORIENTED_EDGE ( 'NONE', *, *, #720, .T. ) ;
#5148 = CARTESIAN_POINT ( 'NONE',  ( -725.0000000000001137, 129.9999999999995453, 4.999999999999999112 ) ) ;
#5149 = ORIENTED_EDGE ( 'NONE', *, *, #14530, .T. ) ;
#5150 = CARTESIAN_POINT ( 'NONE',  ( -80.00000000000002842, 146.6227766016838245, -12.99999999999999822 ) ) ;
#5151 = DIRECTION ( 'NONE',  ( -1.000000000000000000, 0.000000000000000000, 0.000000000000000000 ) ) ;
#5152 = ORIENTED_EDGE ( 'NONE', *, *, #13297, .T. ) ;
#5153 = DIRECTION ( 'NONE',  ( 0.000000000000000000, 1.000000000000000000, 0.000000000000000000 ) ) ;
#5154 = CARTESIAN_POINT ( 'NONE',  ( 24.34257225596280350, 140.5456842492515932, 11.13195485280035513 ) ) ;
#5155 = ADVANCED_FACE ( 'NONE', ( #14441 ), #898, .T. ) ;
#5156 = EDGE_LOOP ( 'NONE', ( #15530, #2469 ) ) ;
#5157 = EDGE_CURVE ( 'NONE', #152, #10357, #1560, .T. ) ;
#5158 = DIRECTION ( 'NONE',  ( -1.000000000000000000, 0.000000000000000000, 0.000000000000000000 ) ) ;
#5159 = EDGE_CURVE ( 'NONE', #7694, #10746, #11450, .T. ) ;
#5160 = ORIENTED_EDGE ( 'NONE', *, *, #9048, .F. ) ;
#5161 = DIRECTION ( 'NONE',  ( 0.000000000000000000, 1.000000000000000000, 0.000000000000000000 ) ) ;
#5162 = DIRECTION ( 'NONE',  ( 1.000000000000000000, 0.000000000000000000, 0.000000000000000000 ) ) ;
#5163 = DIRECTION ( 'NONE',  ( 0.000000000000000000, 0.000000000000000000, 1.000000000000000000 ) ) ;
#5164 = CARTESIAN_POINT ( 'NONE',  ( -15.09627865792072576, 32.41573384469808161, -9.048329374498470301 ) ) ;
#5165 = ORIENTED_EDGE ( 'NONE', *, *, #5384, .F. ) ;
#5166 = DIRECTION ( 'NONE',  ( 0.000000000000000000, 0.000000000000000000, 1.000000000000000000 ) ) ;
#5167 = ORIENTED_EDGE ( 'NONE', *, *, #987, .F. ) ;
#5168 = CARTESIAN_POINT ( 'NONE',  ( 29.78045647795447692, 190.6224931067073669, -29.39406016266897836 ) ) ;
#5169 = CARTESIAN_POINT ( 'NONE',  ( -80.00000000000001421, 196.6227766016838245, -13.00000000000000000 ) ) ;
#5170 = ORIENTED_EDGE ( 'NONE', *, *, #7736, .F. ) ;
#5171 = EDGE_LOOP ( 'NONE', ( #6592, #2361, #16013, #15183 ) ) ;
#5172 = ORIENTED_EDGE ( 'NONE', *, *, #16829, .F. ) ;
#5173 = ADVANCED_FACE ( 'NONE', ( #6711, #6345 ), #14415, .T. ) ;
#5174 = CARTESIAN_POINT ( 'NONE',  ( -72.52785494716455617, 147.3844239155462503, -22.40167687543583952 ) ) ;
#5175 = ORIENTED_EDGE ( 'NONE', *, *, #11335, .T. ) ;
#5176 = CARTESIAN_POINT ( 'NONE',  ( -16.30611068361785954, 32.76923076923075939, 5.287877769756280877 ) ) ;
#5177 = CARTESIAN_POINT ( 'NONE',  ( -13.77790586189935951, 31.39781009804136502, 13.10675149387370197 ) ) ;
#5178 = DIRECTION ( 'NONE',  ( 0.000000000000000000, -1.000000000000000000, 0.000000000000000000 ) ) ;
#5179 = CARTESIAN_POINT ( 'NONE',  ( 22.51491806150639974, 29.85019096660411364, 7.572044396946283840 ) ) ;
#5180 = CARTESIAN_POINT ( 'NONE',  ( 39.99999999999998579, 4.000000000000000000, 33.00000000000000711 ) ) ;
#5181 = VERTEX_POINT ( 'NONE', #11832 ) ;
#5182 = CARTESIAN_POINT ( 'NONE',  ( 2.426025403784448642, 2.655529440325959183E-32, -2.168404344971008868E-16 ) ) ;
#5183 = CARTESIAN_POINT ( 'NONE',  ( 50.00000000000000000, 146.6227766016838245, 0.000000000000000000 ) ) ;
#5184 = CARTESIAN_POINT ( 'NONE',  ( 8.750829511962136209, 133.4309389808502715, 14.69696305399116198 ) ) ;
#5185 = CARTESIAN_POINT ( 'NONE',  ( 40.00000000000000711, 171.6227766016838245, 0.000000000000000000 ) ) ;
#5186 = CARTESIAN_POINT ( 'NONE',  ( -26.11264420168842904, 19.99999999999999645, -13.35921939055851482 ) ) ;
#5187 = ORIENTED_EDGE ( 'NONE', *, *, #7943, .T. ) ;
#5188 = DIRECTION ( 'NONE',  ( 0.000000000000000000, 0.000000000000000000, -1.000000000000000000 ) ) ;
#5189 = EDGE_CURVE ( 'NONE', #14597, #8505, #13718, .T. ) ;
#5190 = CARTESIAN_POINT ( 'NONE',  ( 27.99999999999998224, 9.999999999999998224, -35.00000000000000000 ) ) ;
#5191 = EDGE_LOOP ( 'NONE', ( #9064, #9073, #1208, #3714, #840, #4469 ) ) ;
#5192 = FACE_OUTER_BOUND ( 'NONE', #4697, .T. ) ;
#5193 = DIRECTION ( 'NONE',  ( -1.000000000000000000, 0.000000000000000000, 0.000000000000000000 ) ) ;
#5194 = ORIENTED_EDGE ( 'NONE', *, *, #4185, .F. ) ;
#5195 = DIRECTION ( 'NONE',  ( -1.000000000000000000, 0.000000000000000000, 0.000000000000000000 ) ) ;
#5196 = CARTESIAN_POINT ( 'NONE',  ( 30.00000000000001066, 146.6227766016838245, -16.00000000000000000 ) ) ;
#5197 = CARTESIAN_POINT ( 'NONE',  ( -79.86026353984452442, 140.6228917578588664, -16.24829651775491257 ) ) ;
#5198 = DIRECTION ( 'NONE',  ( 1.000000000000000000, 0.000000000000000000, 0.000000000000000000 ) ) ;
#5199 = ORIENTED_EDGE ( 'NONE', *, *, #16103, .T. ) ;
#5200 = DIRECTION ( 'NONE',  ( 1.000000000000000000, 0.000000000000000000, 0.000000000000000000 ) ) ;
#5201 = FACE_BOUND ( 'NONE', #17199, .T. ) ;
#5202 = LINE ( 'NONE', #3891, #8197 ) ;
#5203 = UNCERTAINTY_MEASURE_WITH_UNIT (LENGTH_MEASURE( 1.000000000000000082E-05 ), #2996, 'distance_accuracy_value', 'NONE');
#5204 = SURFACE_STYLE_USAGE ( .BOTH. , #14851 ) ;
#5205 = ORIENTED_EDGE ( 'NONE', *, *, #114, .F. ) ;
#5206 = EDGE_CURVE ( 'NONE', #6576, #10977, #13435, .T. ) ;
#5207 = ORIENTED_EDGE ( 'NONE', *, *, #13621, .T. ) ;
#5208 = AXIS2_PLACEMENT_3D ( 'NONE', #1136, #12525, #1402 ) ;
#5209 = FACE_OUTER_BOUND ( 'NONE', #14991, .T. ) ;
#5210 = AXIS2_PLACEMENT_3D ( 'NONE', #11782, #4093, #5153 ) ;
#5211 = ORIENTED_EDGE ( 'NONE', *, *, #11134, .T. ) ;
#5212 = FACE_OUTER_BOUND ( 'NONE', #4889, .T. ) ;
#5213 = CARTESIAN_POINT ( 'NONE',  ( 13.82444641086477866, 138.9325364249946517, -8.217559156359119044 ) ) ;
#5214 = ORIENTED_EDGE ( 'NONE', *, *, #13567, .T. ) ;
#5215 = DIRECTION ( 'NONE',  ( -0.000000000000000000, -0.000000000000000000, -1.000000000000000000 ) ) ;
#5216 = CARTESIAN_POINT ( 'NONE',  ( -3.000000000000002665, 171.6227766016838245, 0.000000000000000000 ) ) ;
#5217 = EDGE_CURVE ( 'NONE', #6709, #12804, #718, .T. ) ;
#5218 = EDGE_CURVE ( 'NONE', #13962, #11970, #9832, .T. ) ;
#5219 = LINE ( 'NONE', #9454, #15210 ) ;
#5220 = LINE ( 'NONE', #10617, #1605 ) ;
#5221 = DIRECTION ( 'NONE',  ( -1.000000000000000000, 0.000000000000000000, 0.000000000000000000 ) ) ;
#5222 = AXIS2_PLACEMENT_3D ( 'NONE', #12160, #8164, #12417 ) ;
#5223 = CARTESIAN_POINT ( 'NONE',  ( 18.26135686777330136, 17.99999999999999289, -12.35203162874035065 ) ) ;
#5224 = DIRECTION ( 'NONE',  ( 0.000000000000000000, 1.387778780781445676E-14, 1.000000000000000000 ) ) ;
#5225 = DIRECTION ( 'NONE',  ( 0.000000000000000000, 0.000000000000000000, -1.000000000000000000 ) ) ;
#5226 = VECTOR ( 'NONE', #15146, 1000.000000000000000 ) ;
#5227 = CYLINDRICAL_SURFACE ( 'NONE', #3807, 10.00000000000000178 ) ;
#5228 = PLANE ( 'NONE',  #10865 ) ;
#5229 = ORIENTED_EDGE ( 'NONE', *, *, #16538, .T. ) ;
#5230 = DIRECTION ( 'NONE',  ( 1.000000000000000000, 0.000000000000000000, -0.000000000000000000 ) ) ;
#5231 = DIRECTION ( 'NONE',  ( 0.000000000000000000, 0.000000000000000000, 1.000000000000000000 ) ) ;
#5232 = ORIENTED_EDGE ( 'NONE', *, *, #1257, .T. ) ;
#5233 = DIRECTION ( 'NONE',  ( 0.000000000000000000, 1.000000000000000000, 0.000000000000000000 ) ) ;
#5234 = LINE ( 'NONE', #10633, #16593 ) ;
#5235 = ORIENTED_EDGE ( 'NONE', *, *, #9481, .T. ) ;
#5236 = FACE_OUTER_BOUND ( 'NONE', #1864, .T. ) ;
#5237 = CARTESIAN_POINT ( 'NONE',  ( 15.12922779335904977, 126.1891464972476911, 7.145555214655046505 ) ) ;
#5238 = ORIENTED_EDGE ( 'NONE', *, *, #6965, .F. ) ;
#5239 = CARTESIAN_POINT ( 'NONE',  ( 14.93242934743711814, 30.00000000000000000, 15.00000000000000000 ) ) ;
#5240 = AXIS2_PLACEMENT_3D ( 'NONE', #17163, #4695, #8646 ) ;
#5241 = VECTOR ( 'NONE', #10795, 1000.000000000000000 ) ;
#5242 = VERTEX_POINT ( 'NONE', #12013 ) ;
#5243 = CARTESIAN_POINT ( 'NONE',  ( 31.13499951972123014, 189.1866491494220384, -27.93804624201380804 ) ) ;
#5244 = CARTESIAN_POINT ( 'NONE',  ( 17.56962100350864375, 125.3109322897003608, -3.333333333333324600 ) ) ;
#5245 = CARTESIAN_POINT ( 'NONE',  ( -12.76199592490470636, 18.00000000000464340, -6.193401609026034649 ) ) ;
#5246 = VERTEX_POINT ( 'NONE', #17147 ) ;
#5247 = CARTESIAN_POINT ( 'NONE',  ( 34.06272495246724930, 149.5415222133261466, 24.52446659945426433 ) ) ;
#5248 = ADVANCED_FACE ( 'NONE', ( #3703 ), #6537, .T. ) ;
#5249 = EDGE_CURVE ( 'NONE', #12504, #5356, #17328, .T. ) ;
#5250 = AXIS2_PLACEMENT_3D ( 'NONE', #10498, #4052, #1295 ) ;
#5251 = VERTEX_POINT ( 'NONE', #3882 ) ;
#5252 = CARTESIAN_POINT ( 'NONE',  ( -81.45415618582130435, 189.2596037578064454, -27.89172594985640430 ) ) ;
#5253 = DIRECTION ( 'NONE',  ( -0.000000000000000000, -0.000000000000000000, -1.000000000000000000 ) ) ;
#5254 = VECTOR ( 'NONE', #3543, 1000.000000000000000 ) ;
#5255 = VERTEX_POINT ( 'NONE', #14677 ) ;
#5256 = VERTEX_POINT ( 'NONE', #2554 ) ;
#5257 = ORIENTED_EDGE ( 'NONE', *, *, #4986, .T. ) ;
#5258 = CARTESIAN_POINT ( 'NONE',  ( 27.48361012698979522, 126.6227766016837819, -6.072704737864100906E-13 ) ) ;
#5259 = CLOSED_SHELL ( 'NONE', ( #11395, #10558, #4241, #14247, #4405, #5362, #4362, #7058, #3636, #8631 ) ) ;
#5260 = VECTOR ( 'NONE', #11788, 1000.000000000000000 ) ;
#5261 = ORIENTED_EDGE ( 'NONE', *, *, #4841, .T. ) ;
#5262 = CARTESIAN_POINT ( 'NONE',  ( -15.77503540472913457, 32.61497647743762229, 7.787339510197840653 ) ) ;
#5263 = VECTOR ( 'NONE', #15882, 1000.000000000000000 ) ;
#5264 = FILL_AREA_STYLE_COLOUR ( '', #16842 ) ;
#5265 = CARTESIAN_POINT ( 'NONE',  ( 24.00000000000000355, 146.9394831494156790, -24.81813469455734378 ) ) ;
#5266 = CARTESIAN_POINT ( 'NONE',  ( 32.50000000000000000, 196.6227766016838245, 0.000000000000000000 ) ) ;
#5267 = DIRECTION ( 'NONE',  ( -1.000000000000000000, -0.000000000000000000, -0.000000000000000000 ) ) ;
#5268 = VERTEX_POINT ( 'NONE', #13352 ) ;
#5269 = CARTESIAN_POINT ( 'NONE',  ( 27.99999999999998224, 9.999999999999998224, 10.00000000000000178 ) ) ;
#5270 = CARTESIAN_POINT ( 'NONE',  ( 24.93507336697353338, 29.86842105263157521, -5.660390792616599498 ) ) ;
#5271 = EDGE_CURVE ( 'NONE', #3217, #5676, #17416, .T. ) ;
#5272 = ADVANCED_FACE ( 'NONE', ( #5387 ), #10944, .F. ) ;
#5273 = CARTESIAN_POINT ( 'NONE',  ( 15.00000000000903455, 143.2058235767352983, -16.77804593520375676 ) ) ;
#5274 = EDGE_CURVE ( 'NONE', #1367, #12793, #7222, .T. ) ;
#5275 = PLANE ( 'NONE',  #7752 ) ;
#5276 = CARTESIAN_POINT ( 'NONE',  ( 21.54624641763228254, 29.91220938647573391, 12.53033468027509478 ) ) ;
#5277 = EDGE_CURVE ( 'NONE', #10995, #11591, #15192, .T. ) ;
#5278 = ORIENTED_EDGE ( 'NONE', *, *, #6382, .F. ) ;
#5279 = CARTESIAN_POINT ( 'NONE',  ( -85.27494917608791525, 141.2912748254776147, -13.00000000000000000 ) ) ;
#5280 = AXIS2_PLACEMENT_3D ( 'NONE', #1776, #1863, #3456 ) ;
#5281 = AXIS2_PLACEMENT_3D ( 'NONE', #13290, #11448, #2483 ) ;
#5282 = STYLED_ITEM ( 'NONE', ( #1212 ), #12908 ) ;
#5283 = VECTOR ( 'NONE', #9283, 1000.000000000000000 ) ;
#5284 = CARTESIAN_POINT ( 'NONE',  ( 15.00000000000000000, 143.0344144757318929, 16.50549856913627877 ) ) ;
#5285 = DIRECTION ( 'NONE',  ( 1.156482317317868274E-16, -1.000000000000000000, 0.000000000000000000 ) ) ;
#5286 = APPLICATION_CONTEXT ( 'automotive_design' ) ;
#5287 = EDGE_LOOP ( 'NONE', ( #7055, #14522, #9950, #15928 ) ) ;
#5288 = SURFACE_STYLE_FILL_AREA ( #6263 ) ;
#5289 = VERTEX_POINT ( 'NONE', #9436 ) ;
#5290 = CARTESIAN_POINT ( 'NONE',  ( -100.0000000000000000, 144.1839557653416080, -18.33333333333335702 ) ) ;
#5291 = CARTESIAN_POINT ( 'NONE',  ( 16.61976933981454962, 29.96600215813370838, -12.82127072618890118 ) ) ;
#5292 = CARTESIAN_POINT ( 'NONE',  ( -48.00000000000000000, 154.3022685259950038, -9.999999999999900524 ) ) ;
#5293 = VECTOR ( 'NONE', #15572, 1000.000000000000000 ) ;
#5294 = EDGE_CURVE ( 'NONE', #11801, #1199, #2702, .T. ) ;
#5295 = CARTESIAN_POINT ( 'NONE',  ( 27.30499999999999616, 0.000000000000000000, 0.000000000000000000 ) ) ;
#5296 = CIRCLE ( 'NONE', #3315, 5.000000000000004441 ) ;
#5297 = ORIENTED_EDGE ( 'NONE', *, *, #2145, .F. ) ;
#5298 = DIRECTION ( 'NONE',  ( 0.000000000000000000, 0.000000000000000000, 1.000000000000000000 ) ) ;
#5299 = DIRECTION ( 'NONE',  ( -0.000000000000000000, -0.000000000000000000, -1.000000000000000000 ) ) ;
#5300 = DIRECTION ( 'NONE',  ( -0.9940220915700700433, -0.05458956280889060153, 0.09455189634796991316 ) ) ;
#5301 = B_SPLINE_CURVE_WITH_KNOTS ( 'NONE', 3,
 ( #10250, #16005, #17069, #7856 ),
 .UNSPECIFIED., .F., .F.,
 ( 4, 4 ),
 ( 0.000000000000000000, 0.001170341053039947524 ),
 .UNSPECIFIED. ) ;
#5302 = DIRECTION ( 'NONE',  ( 1.000000000000000000, -0.000000000000000000, -0.000000000000000000 ) ) ;
#5303 = PRODUCT_DEFINITION_CONTEXT ( 'detailed design', #5286, 'design' ) ;
#5304 = ORIENTED_EDGE ( 'NONE', *, *, #15386, .T. ) ;
#5305 = CARTESIAN_POINT ( 'NONE',  ( 0.000000000000000000, 18.00000000000000355, 25.00000000000000000 ) ) ;
#5306 = AXIS2_PLACEMENT_3D ( 'NONE', #9251, #4847, #8988 ) ;
#5307 = EDGE_LOOP ( 'NONE', ( #16447, #15426, #9108, #10380, #617, #10194, #13742, #17512, #16882, #10842, #6434, #15902 ) ) ;
#5308 = CARTESIAN_POINT ( 'NONE',  ( -83.53742222559971253, 151.4735692324751994, -28.61877689333859109 ) ) ;
#5309 = VECTOR ( 'NONE', #17172, 1000.000000000000000 ) ;
#5310 = CARTESIAN_POINT ( 'NONE',  ( 14.28882419134376747, 138.6263508161794675, -3.987386623658401241 ) ) ;
#5311 = ORIENTED_EDGE ( 'NONE', *, *, #6514, .T. ) ;
#5312 = FACE_OUTER_BOUND ( 'NONE', #10473, .T. ) ;
#5313 = DIRECTION ( 'NONE',  ( -0.000000000000000000, -1.000000000000000000, -0.000000000000000000 ) ) ;
#5314 = MANIFOLD_SOLID_BREP ( 'Fillet1', #1585 ) ;
#5315 = FACE_OUTER_BOUND ( 'NONE', #7371, .T. ) ;
#5316 = ADVANCED_FACE ( 'NONE', ( #8375 ), #12367, .T. ) ;
#5317 = DIRECTION ( 'NONE',  ( 1.000000000000000000, 0.000000000000000000, 0.000000000000000000 ) ) ;
#5318 = ADVANCED_FACE ( 'NONE', ( #405 ), #7059, .F. ) ;
#5319 = CARTESIAN_POINT ( 'NONE',  ( -167.6513770290094385, 174.2473783649210759, 4.898587196589412829E-16 ) ) ;
#5320 = CARTESIAN_POINT ( 'NONE',  ( 19.87492423018547427, 17.99999999999543121, -11.43634947295695703 ) ) ;
#5321 = CARTESIAN_POINT ( 'NONE',  ( -91.33974596215564645, 171.6227766016838245, 0.000000000000000000 ) ) ;
#5322 = FACE_OUTER_BOUND ( 'NONE', #1370, .T. ) ;
#5323 = CIRCLE ( 'NONE', #7012, 2.500000000000002220 ) ;
#5324 = DIRECTION ( 'NONE',  ( 0.000000000000000000, 1.000000000000000000, 0.000000000000000000 ) ) ;
#5325 = AXIS2_PLACEMENT_3D ( 'NONE', #1680, #2913, #8570 ) ;
#5326 = CARTESIAN_POINT ( 'NONE',  ( 32.50000000000000711, 146.6227766016838245, 0.000000000000000000 ) ) ;
#5327 = ORIENTED_EDGE ( 'NONE', *, *, #345, .T. ) ;
#5328 = CARTESIAN_POINT ( 'NONE',  ( -25.00000000000002132, 130.0000000000000000, 15.00000000000000000 ) ) ;
#5329 = ORIENTED_EDGE ( 'NONE', *, *, #4352, .F. ) ;
#5330 = LINE ( 'NONE', #7979, #8466 ) ;
#5331 = EDGE_CURVE ( 'NONE', #12122, #15415, #150, .T. ) ;
#5332 = CARTESIAN_POINT ( 'NONE',  ( 0.000000000000000000, 0.000000000000000000, 0.000000000000000000 ) ) ;
#5333 = ORIENTED_EDGE ( 'NONE', *, *, #9719, .T. ) ;
#5334 = CARTESIAN_POINT ( 'NONE',  ( -10.59078875499043981, 20.00000000000000000, 13.69642986623834702 ) ) ;
#5335 = CARTESIAN_POINT ( 'NONE',  ( -125.0000000000000000, 206.6227766016838245, 0.000000000000000000 ) ) ;
#5336 = EDGE_LOOP ( 'NONE', ( #5648, #9144, #4783, #8908, #1418, #4694 ) ) ;
#5337 = DIRECTION ( 'NONE',  ( 0.000000000000000000, 0.000000000000000000, 1.000000000000000000 ) ) ;
#5338 = CONICAL_SURFACE ( 'NONE', #4495, 8.000000000000007105, 0.08726646259970990971 ) ;
#5339 = ORIENTED_EDGE ( 'NONE', *, *, #8939, .T. ) ;
#5340 = CARTESIAN_POINT ( 'NONE',  ( -34.99999999999999289, 122.0000000000000284, 4.999999999999999112 ) ) ;
#5341 = CARTESIAN_POINT ( 'NONE',  ( 36.97967542706143718, 193.8447098639589967, -24.40281628369250555 ) ) ;
#5342 = DIRECTION ( 'NONE',  ( 1.000000000000000000, 0.000000000000000000, -0.000000000000000000 ) ) ;
#5343 = PLANE ( 'NONE',  #8037 ) ;
#5344 = ORIENTED_EDGE ( 'NONE', *, *, #13274, .T. ) ;
#5345 = SHAPE_REPRESENTATION ( 'torque adjustment ring', ( #3583 ), #17150 ) ;
#5346 = CARTESIAN_POINT ( 'NONE',  ( 34.89689726072227671, 147.6679082027615948, 22.70058015389365735 ) ) ;
#5347 = AXIS2_PLACEMENT_3D ( 'NONE', #12562, #16738, #9906 ) ;
#5348 = VECTOR ( 'NONE', #4483, 1000.000000000000000 ) ;
#5349 = ORIENTED_EDGE ( 'NONE', *, *, #3481, .F. ) ;
#5350 = CARTESIAN_POINT ( 'NONE',  ( -87.50000000000004263, 196.2479045481292985, -21.97573418327510808 ) ) ;
#5351 = TOROIDAL_SURFACE ( 'NONE', #1396, 2.699999999999999289, 0.2000000000000000111 ) ;
#5352 = CARTESIAN_POINT ( 'NONE',  ( -90.80384757729339640, 138.6227766016838245, 0.000000000000000000 ) ) ;
#5353 = EDGE_CURVE ( 'NONE', #11033, #11867, #329, .T. ) ;
#5354 = VERTEX_POINT ( 'NONE', #12460 ) ;
#5355 = ORIENTED_EDGE ( 'NONE', *, *, #9268, .F. ) ;
#5356 = VERTEX_POINT ( 'NONE', #14842 ) ;
#5357 = B_SPLINE_CURVE_WITH_KNOTS ( 'NONE', 3,
 ( #7171, #7514, #16824, #437, #15491, #4531, #14178, #16660, #804, #9916, #2039, #1950, #16747, #8679, #4612, #538, #14089, #7353, #12834, #7433 ),
 .UNSPECIFIED., .F., .F.,
 ( 4, 2, 2, 2, 2, 2, 2, 2, 2, 4 ),
 ( 0.000000000000000000, 0.002318945972243265704, 0.003478418958364892268, 0.004637891944486519265, 0.006956837916729771525, 0.009275783888973026386, 0.01159472986121627865, 0.01391367583345953091, 0.01623262180570278490, 0.01855156777794603890 ),
 .UNSPECIFIED. ) ;
#5358 = CARTESIAN_POINT ( 'NONE',  ( 7.559396570614633326, 133.9010074147453508, 14.92908841323498770 ) ) ;
#5359 = CIRCLE ( 'NONE', #11011, 30.00000000000000000 ) ;
#5360 = ORIENTED_EDGE ( 'NONE', *, *, #5423, .F. ) ;
#5361 = APPLICATION_PROTOCOL_DEFINITION ( 'draft international standard', 'automotive_design', 1998, #14555 ) ;
#5362 = ADVANCED_FACE ( 'NONE', ( #12200, #15098 ), #11118, .T. ) ;
#5363 = CARTESIAN_POINT ( 'NONE',  ( -725.0000000000000000, 30.00000000000000000, 15.00000000000000000 ) ) ;
#5364 = AXIS2_PLACEMENT_3D ( 'NONE', #7899, #8158, #11784 ) ;
#5365 = FACE_OUTER_BOUND ( 'NONE', #752, .T. ) ;
#5366 = CARTESIAN_POINT ( 'NONE',  ( -90.80384757729339640, 138.6227766016838245, 0.000000000000000000 ) ) ;
#5367 = FACE_BOUND ( 'NONE', #14169, .T. ) ;
#5368 = CARTESIAN_POINT ( 'NONE',  ( -77.93529739263047418, 151.1803749979462737, 25.90597399044991889 ) ) ;
#5369 = ORIENTED_EDGE ( 'NONE', *, *, #11224, .F. ) ;
#5370 = DIRECTION ( 'NONE',  ( -1.000000000000000000, -6.938893903907228378E-16, 0.000000000000000000 ) ) ;
#5371 = CARTESIAN_POINT ( 'NONE',  ( -15.00000000000001421, 130.0000000000000000, 13.00000000000000000 ) ) ;
#5372 = CARTESIAN_POINT ( 'NONE',  ( 49.99999999999998579, 163.6227766016838530, -12.50000337241049309 ) ) ;
#5373 = FACE_OUTER_BOUND ( 'NONE', #5961, .T. ) ;
#5374 = DIRECTION ( 'NONE',  ( -0.08715574274764689711, 0.9961946980917465444, 0.000000000000000000 ) ) ;
#5375 = DIRECTION ( 'NONE',  ( 1.156482317317868274E-16, -1.000000000000000000, 0.000000000000000000 ) ) ;
#5376 = AXIS2_PLACEMENT_3D ( 'NONE', #12829, #1944, #3005 ) ;
#5377 = VECTOR ( 'NONE', #12648, 1000.000000000000000 ) ;
#5378 = CARTESIAN_POINT ( 'NONE',  ( -98.00000000000000000, 171.6227766016838245, 0.000000000000000000 ) ) ;
#5379 = ORIENTED_EDGE ( 'NONE', *, *, #11054, .T. ) ;
#5380 = DIRECTION ( 'NONE',  ( -0.000000000000000000, -0.000000000000000000, -1.000000000000000000 ) ) ;
#5381 = VERTEX_POINT ( 'NONE', #9792 ) ;
#5382 = EDGE_CURVE ( 'NONE', #11298, #9392, #6365, .T. ) ;
#5383 =( NAMED_UNIT ( * ) PLANE_ANGLE_UNIT ( ) SI_UNIT ( $, .RADIAN. ) );
#5384 = EDGE_CURVE ( 'NONE', #11068, #15082, #11463, .T. ) ;
#5385 = CARTESIAN_POINT ( 'NONE',  ( 15.56337975240373872, 125.2134999403456135, -4.999999999999997335 ) ) ;
#5386 = ADVANCED_FACE ( 'NONE', ( #14934 ), #16716, .T. ) ;
#5387 = FACE_OUTER_BOUND ( 'NONE', #3496, .T. ) ;
#5388 = VECTOR ( 'NONE', #5285, 1000.000000000000000 ) ;
#5389 = DIRECTION ( 'NONE',  ( 0.000000000000000000, -0.8660254037844413721, -0.4999999999999953371 ) ) ;
#5390 = AXIS2_PLACEMENT_3D ( 'NONE', #4848, #14229, #7578 ) ;
#5391 = VECTOR ( 'NONE', #676, 1000.000000000000000 ) ;
#5392 = CARTESIAN_POINT ( 'NONE',  ( -26.89314795393037016, 19.99999999999999289, 11.55702759004480207 ) ) ;
#5393 = EDGE_LOOP ( 'NONE', ( #17208, #9508, #4771, #9871, #5684, #8280, #3828, #13692, #589, #11880, #15351, #5311, #9119, #2947, #981, #12948, #13355, #5817, #13278, #11381, #8133, #11283, #8888, #2327, #9325, #9006, #9539, #8043, #11084, #9300, #14532, #6854, #6817, #2408, #7392, #2230, #7306, #2576, #7520, #15188, #9135, #16467, #12753, #10723, #16786, #14080, #3945, #8722, #4952, #1267, #9956, #7867, #5950, #14714, #9375 ) ) ;
#5394 = CYLINDRICAL_SURFACE ( 'NONE', #13214, 2.500000000000000444 ) ;
#5395 = DIRECTION ( 'NONE',  ( -1.000000000000000000, 0.000000000000000000, 0.000000000000000000 ) ) ;
#5396 = DIRECTION ( 'NONE',  ( 0.000000000000000000, 0.000000000000000000, -1.000000000000000000 ) ) ;
#5397 = FILL_AREA_STYLE ('',( #7763 ) ) ;
#5398 = ORIENTED_EDGE ( 'NONE', *, *, #3658, .F. ) ;
#5399 = CARTESIAN_POINT ( 'NONE',  ( 16.12877328687227774, 136.8349817083154676, -4.209125965272636272 ) ) ;
#5400 = ORIENTED_EDGE ( 'NONE', *, *, #8514, .F. ) ;
#5401 = FACE_BOUND ( 'NONE', #7848, .T. ) ;
#5402 = VECTOR ( 'NONE', #7384, 1000.000000000000000 ) ;
#5403 = DIRECTION ( 'NONE',  ( -1.000000000000000000, 0.000000000000000000, 0.000000000000000000 ) ) ;
#5404 = VERTEX_POINT ( 'NONE', #5907 ) ;
#5405 = DIRECTION ( 'NONE',  ( 1.000000000000000000, 0.000000000000000000, 0.000000000000000000 ) ) ;
#5406 = DIRECTION ( 'NONE',  ( 0.000000000000000000, 0.000000000000000000, 1.000000000000000000 ) ) ;
#5407 = MANIFOLD_SOLID_BREP ( 'Fillet2', #5259 ) ;
#5408 = CARTESIAN_POINT ( 'NONE',  ( 23.34636706823183872, 200.1176944260899120, -16.66575456205188743 ) ) ;
#5409 = DIRECTION ( 'NONE',  ( -0.000000000000000000, -0.000000000000000000, -1.000000000000000000 ) ) ;
#5410 = CARTESIAN_POINT ( 'NONE',  ( 0.000000000000000000, 0.000000000000000000, 2.499999999999999112 ) ) ;
#5411 = CARTESIAN_POINT ( 'NONE',  ( 18.93266870823487125, 29.92002005853035840, -11.93384102663519997 ) ) ;
#5412 = CARTESIAN_POINT ( 'NONE',  ( -22.99999999999999289, 100.0000000000000142, 0.000000000000000000 ) ) ;
#5413 = CIRCLE ( 'NONE', #4568, 5.999999999999998224 ) ;
#5414 = CARTESIAN_POINT ( 'NONE',  ( -103.0000000000000142, 171.6227766016838245, -5.000000000000007994 ) ) ;
#5415 = CARTESIAN_POINT ( 'NONE',  ( -50.00000000000000000, 154.3022685259950038, -9.999999999999900524 ) ) ;
#5416 = CARTESIAN_POINT ( 'NONE',  ( 27.59653005489939659, 141.1206502181308338, -17.16533225383574290 ) ) ;
#5417 = VERTEX_POINT ( 'NONE', #7227 ) ;
#5418 = CARTESIAN_POINT ( 'NONE',  ( 8.750829511962136209, 133.4309389808502715, -14.69696305399116198 ) ) ;
#5419 = ORIENTED_EDGE ( 'NONE', *, *, #10825, .T. ) ;
#5420 = CARTESIAN_POINT ( 'NONE',  ( -20.00000000000000355, 171.6227766016838245, 0.000000000000000000 ) ) ;
#5421 = CARTESIAN_POINT ( 'NONE',  ( -48.00000000000000000, 171.6227766016838245, 0.000000000000000000 ) ) ;
#5422 = ORIENTED_EDGE ( 'NONE', *, *, #10511, .T. ) ;
#5423 = EDGE_CURVE ( 'NONE', #7078, #12240, #12979, .T. ) ;
#5424 = CARTESIAN_POINT ( 'NONE',  ( -10.16681828783789143, 30.62365918355438055, 14.67566226953583985 ) ) ;
#5425 = CARTESIAN_POINT ( 'NONE',  ( 22.72753210816364700, 141.1551838527312555, 12.68377836492884470 ) ) ;
#5426 = AXIS2_PLACEMENT_3D ( 'NONE', #1787, #2934, #7102 ) ;
#5427 = VERTEX_POINT ( 'NONE', #501 ) ;
#5428 = CARTESIAN_POINT ( 'NONE',  ( 16.23725950538873164, 20.00000000000000000, 24.99999999984155252 ) ) ;
#5429 = ORIENTED_EDGE ( 'NONE', *, *, #12280, .T. ) ;
#5430 = DIRECTION ( 'NONE',  ( -0.000000000000000000, -0.000000000000000000, 1.000000000000000000 ) ) ;
#5431 = PLANE ( 'NONE',  #10027 ) ;
#5432 = DIRECTION ( 'NONE',  ( -1.000000000000000000, -0.000000000000000000, 0.000000000000000000 ) ) ;
#5433 = CARTESIAN_POINT ( 'NONE',  ( -208.3486229709906468, 168.0754701982166068, -6.144114920819718328 ) ) ;
#5434 = ORIENTED_EDGE ( 'NONE', *, *, #8492, .F. ) ;
#5435 = DIRECTION ( 'NONE',  ( 0.000000000000000000, 0.000000000000000000, 1.000000000000000000 ) ) ;
#5436 = ORIENTED_EDGE ( 'NONE', *, *, #7524, .T. ) ;
#5437 = CARTESIAN_POINT ( 'NONE',  ( -79.43652167955697507, 189.1215240515805931, -27.97845313684487678 ) ) ;
#5438 = LINE ( 'NONE', #11086, #7247 ) ;
#5439 = ORIENTED_EDGE ( 'NONE', *, *, #15638, .F. ) ;
#5440 = VERTEX_POINT ( 'NONE', #6072 ) ;
#5441 = ORIENTED_EDGE ( 'NONE', *, *, #6741, .F. ) ;
#5442 = EDGE_CURVE ( 'NONE', #2002, #5792, #12890, .T. ) ;
#5443 = CARTESIAN_POINT ( 'NONE',  ( -68.00000000000000000, 143.0439382767972347, 16.49999999999984368 ) ) ;
#5444 = B_SPLINE_CURVE_WITH_KNOTS ( 'NONE', 3,
 ( #1116, #5270, #3688, #16084, #7931, #15982, #14753, #1291, #10673, #11722, #5101, #14661, #15898, #16177, #6604, #940, #3961, #9346, #2348, #2625, #9075, #7662, #13337, #13151, #11817 ),
 .UNSPECIFIED., .F., .F.,
 ( 4, 2, 2, 2, 2, 2, 2, 2, 2, 1, 2, 2, 4 ),
 ( 0.000000000000000000, 0.001953037758357041142, 0.002929556637535561930, 0.003906075516714082284, 0.005859113275071132533, 0.006835632154249659392, 0.007812151033428187119, 0.009765188791785242572, 0.01074170767096376509, 0.01171822655014228762, 0.01269474542932080841, 0.01367126430849933093, 0.01562430206685638465 ),
 .UNSPECIFIED. ) ;
#5445 = EDGE_CURVE ( 'NONE', #8820, #12504, #12807, .T. ) ;
#5446 = VERTEX_POINT ( 'NONE', #15365 ) ;
#5447 = CARTESIAN_POINT ( 'NONE',  ( -30.49999999999998224, 10.00000000000000000, 1.387778780781445676E-14 ) ) ;
#5448 = ADVANCED_FACE ( 'NONE', ( #15626 ), #4583, .F. ) ;
#5449 = CARTESIAN_POINT ( 'NONE',  ( -27.99999999999998224, 10.00000000000000000, -35.00200000000000244 ) ) ;
#5450 = EDGE_CURVE ( 'NONE', #11548, #2095, #8428, .T. ) ;
#5451 = FACE_OUTER_BOUND ( 'NONE', #14740, .T. ) ;
#5452 = DIRECTION ( 'NONE',  ( 1.000000000000000000, 0.000000000000000000, 0.000000000000000000 ) ) ;
#5453 = CARTESIAN_POINT ( 'NONE',  ( -83.42148544384103559, 150.2853719096988812, 25.17531865327014629 ) ) ;
#5454 = ORIENTED_EDGE ( 'NONE', *, *, #7249, .F. ) ;
#5455 = CARTESIAN_POINT ( 'NONE',  ( -79.06135944198280185, 202.5503328113395298, -16.38559373769483685 ) ) ;
#5456 = CARTESIAN_POINT ( 'NONE',  ( 11.07991637643875116, 132.1496266960828336, 13.91448104906911709 ) ) ;
#5457 = DIRECTION ( 'NONE',  ( 0.000000000000000000, 0.000000000000000000, -1.000000000000000000 ) ) ;
#5458 = DIRECTION ( 'NONE',  ( 1.000000000000000000, 0.000000000000000000, 0.000000000000000000 ) ) ;
#5459 = DIRECTION ( 'NONE',  ( -0.000000000000000000, -0.000000000000000000, -1.000000000000000000 ) ) ;
#5460 = EDGE_CURVE ( 'NONE', #1799, #7907, #8890, .T. ) ;
#5461 = CARTESIAN_POINT ( 'NONE',  ( -90.80384757729339640, 138.6227766016838245, 0.000000000000000000 ) ) ;
#5462 = ORIENTED_EDGE ( 'NONE', *, *, #10405, .F. ) ;
#5463 = DIRECTION ( 'NONE',  ( 1.000000000000000000, 0.000000000000000000, 0.000000000000000000 ) ) ;
#5464 = VERTEX_POINT ( 'NONE', #15892 ) ;
#5465 = CARTESIAN_POINT ( 'NONE',  ( 27.48361012695778882, 136.6227766016838530, -1.300194169143111589 ) ) ;
#5466 = CARTESIAN_POINT ( 'NONE',  ( 49.99999999999998579, 179.6227766016838245, -12.50000337241049309 ) ) ;
#5467 = CARTESIAN_POINT ( 'NONE',  ( -82.50000000000002842, 146.6227766016838245, 0.000000000000000000 ) ) ;
#5468 = DIRECTION ( 'NONE',  ( -1.000000000000000000, -0.000000000000000000, -0.000000000000000000 ) ) ;
#5469 = VERTEX_POINT ( 'NONE', #6416 ) ;
#5470 = CARTESIAN_POINT ( 'NONE',  ( 40.00000000000000711, 146.6227766016838245, 0.000000000000000000 ) ) ;
#5471 = CARTESIAN_POINT ( 'NONE',  ( -27.99999999999998224, 10.00000000000000000, -12.99999999999999822 ) ) ;
#5472 = FACE_OUTER_BOUND ( 'NONE', #10269, .T. ) ;
#5473 = CARTESIAN_POINT ( 'NONE',  ( 49.99999999999998579, 175.6227766016838245, 8.071800142134975431 ) ) ;
#5474 = EDGE_CURVE ( 'NONE', #7978, #14499, #14574, .T. ) ;
#5475 = EDGE_CURVE ( 'NONE', #7915, #14615, #17044, .T. ) ;
#5476 = EDGE_CURVE ( 'NONE', #3210, #7898, #931, .T. ) ;
#5477 = CARTESIAN_POINT ( 'NONE',  ( 16.36928288456664049, 136.8619714623083610, -5.700917076122243188 ) ) ;
#5478 = ORIENTED_EDGE ( 'NONE', *, *, #16537, .F. ) ;
#5479 = CARTESIAN_POINT ( 'NONE',  ( -74.09965740015987024, 147.9183216992699101, -25.76577836882853489 ) ) ;
#5480 = CARTESIAN_POINT ( 'NONE',  ( -50.00000000000000711, -20.00000000000000000, 40.00000000000000711 ) ) ;
#5481 = VERTEX_POINT ( 'NONE', #6321 ) ;
#5482 = CARTESIAN_POINT ( 'NONE',  ( 0.000000000000000000, 0.000000000000000000, 0.000000000000000000 ) ) ;
#5483 = CARTESIAN_POINT ( 'NONE',  ( -25.00000000000002132, 120.0000000000000284, 5.000000000000023093 ) ) ;
#5484 = MANIFOLD_SOLID_BREP ( 'CirPattern1[2]', #16287 ) ;
#5485 = FACE_OUTER_BOUND ( 'NONE', #13933, .T. ) ;
#5486 = CARTESIAN_POINT ( 'NONE',  ( 24.99999999999999645, 196.1091490972146403, 22.13677318565946095 ) ) ;
#5487 = CARTESIAN_POINT ( 'NONE',  ( 33.66231827095856488, 18.00000000000000000, -12.04861179558545636 ) ) ;
#5488 = CARTESIAN_POINT ( 'NONE',  ( 20.77386775082738879, 29.88392224133981401, -10.47448535043027462 ) ) ;
#5489 = DIRECTION ( 'NONE',  ( 0.000000000000000000, 0.000000000000000000, 1.000000000000000000 ) ) ;
#5490 = DIRECTION ( 'NONE',  ( 1.000000000000000000, 0.000000000000000000, -0.000000000000000000 ) ) ;
#5491 = CARTESIAN_POINT ( 'NONE',  ( 49.99999999999998579, 179.6227766016838245, 10.00000337241049309 ) ) ;
#5492 = DIRECTION ( 'NONE',  ( 0.000000000000000000, 0.000000000000000000, 1.000000000000000000 ) ) ;
#5493 = CIRCLE ( 'NONE', #8308, 3.999999999999998668 ) ;
#5494 = ORIENTED_EDGE ( 'NONE', *, *, #14985, .T. ) ;
#5495 = CARTESIAN_POINT ( 'NONE',  ( 9.788850454972870097, 132.9181049171561995, -14.40474131580982231 ) ) ;
#5496 = EDGE_CURVE ( 'NONE', #6195, #13094, #15975, .T. ) ;
#5497 = EDGE_CURVE ( 'NONE', #1301, #3629, #6525, .T. ) ;
#5498 = AXIS2_PLACEMENT_3D ( 'NONE', #8953, #10011, #4971 ) ;
#5499 = EDGE_LOOP ( 'NONE', ( #13309, #15018, #1023, #14183, #15285, #17226, #15514, #143, #12322, #5349 ) ) ;
#5500 = DIRECTION ( 'NONE',  ( 0.000000000000000000, 0.000000000000000000, 1.000000000000000000 ) ) ;
#5501 = FACE_OUTER_BOUND ( 'NONE', #5171, .T. ) ;
#5502 = ORIENTED_EDGE ( 'NONE', *, *, #7865, .T. ) ;
#5503 = CARTESIAN_POINT ( 'NONE',  ( -13.98869899561406882, 20.00000000000231637, 10.23150106588177621 ) ) ;
#5504 = DIRECTION ( 'NONE',  ( 0.000000000000000000, 1.000000000000000000, 0.000000000000000000 ) ) ;
#5505 = ORIENTED_EDGE ( 'NONE', *, *, #14789, .F. ) ;
#5506 = CARTESIAN_POINT ( 'NONE',  ( 37.50000000000000000, 146.9976486552383790, -21.97573418327510097 ) ) ;
#5507 = VECTOR ( 'NONE', #5958, 1000.000000000000000 ) ;
#5508 = ORIENTED_EDGE ( 'NONE', *, *, #7160, .T. ) ;
#5509 = CARTESIAN_POINT ( 'NONE',  ( -80.00000000000001421, 196.6227766016838245, -12.99999999999999822 ) ) ;
#5510 = FACE_OUTER_BOUND ( 'NONE', #9230, .T. ) ;
#5511 = DIRECTION ( 'NONE',  ( -0.000000000000000000, -0.000000000000000000, 1.000000000000000000 ) ) ;
#5512 = VERTEX_POINT ( 'NONE', #7923 ) ;
#5513 = FACE_BOUND ( 'NONE', #3372, .T. ) ;
#5514 = EDGE_CURVE ( 'NONE', #588, #9872, #17408, .T. ) ;
#5515 = EDGE_LOOP ( 'NONE', ( #5570, #16193, #16050, #7766, #14975, #16631 ) ) ;
#5516 = CARTESIAN_POINT ( 'NONE',  ( 25.00000000000001421, 147.1386660375792417, 22.13939837391653853 ) ) ;
#5517 = APPLICATION_CONTEXT ( 'automotive_design' ) ;
#5518 = ORIENTED_EDGE ( 'NONE', *, *, #3635, .T. ) ;
#5519 = CARTESIAN_POINT ( 'NONE',  ( -85.93543503013836471, 192.0313071030111871, -25.93356563065114528 ) ) ;
#5520 = DIRECTION ( 'NONE',  ( 0.000000000000000000, 0.000000000000000000, -1.000000000000000000 ) ) ;
#5521 = CARTESIAN_POINT ( 'NONE',  ( -15.27350142870561811, 32.46802521863179436, -8.792838265516087048 ) ) ;
#5522 = ORIENTED_EDGE ( 'NONE', *, *, #3593, .T. ) ;
#5523 = VERTEX_POINT ( 'NONE', #17393 ) ;
#5524 = VECTOR ( 'NONE', #2263, 1000.000000000000000 ) ;
#5525 = DIRECTION ( 'NONE',  ( 0.000000000000000000, 0.000000000000000000, 1.000000000000000000 ) ) ;
#5526 = CARTESIAN_POINT ( 'NONE',  ( 9.647168043681871197, 132.9898913927504225, 14.44632387683999575 ) ) ;
#5527 = EDGE_LOOP ( 'NONE', ( #12945, #1451, #5502, #15102 ) ) ;
#5528 = DIRECTION ( 'NONE',  ( 0.000000000000000000, 0.000000000000000000, 1.000000000000000000 ) ) ;
#5529 = CARTESIAN_POINT ( 'NONE',  ( -197.9999999999999716, 171.6227766016838245, 0.000000000000000000 ) ) ;
#5530 = DIRECTION ( 'NONE',  ( 1.000000000000000000, 0.000000000000000000, 0.000000000000000000 ) ) ;
#5531 = CARTESIAN_POINT ( 'NONE',  ( 22.93524650466161674, 29.84210526315774104, -5.528366322421692125 ) ) ;
#5532 = DIRECTION ( 'NONE',  ( -1.000000000000000000, -0.000000000000000000, -0.000000000000000000 ) ) ;
#5533 = LINE ( 'NONE', #4213, #6933 ) ;
#5534 = AXIS2_PLACEMENT_3D ( 'NONE', #15903, #15815, #13156 ) ;
#5535 = EDGE_CURVE ( 'NONE', #13709, #5614, #2955, .T. ) ;
#5536 = VECTOR ( 'NONE', #5267, 1000.000000000000000 ) ;
#5537 = ORIENTED_EDGE ( 'NONE', *, *, #9179, .T. ) ;
#5538 = CARTESIAN_POINT ( 'NONE',  ( -82.39581698594608383, 202.1282835878849369, -17.15932559113869971 ) ) ;
#5539 = CARTESIAN_POINT ( 'NONE',  ( 196.0000000000000000, 163.6227766016838530, -12.50000337241049309 ) ) ;
#5540 = LINE ( 'NONE', #9604, #1271 ) ;
#5541 = CYLINDRICAL_SURFACE ( 'NONE', #4780, 12.00000000000000000 ) ;
#5542 = DIRECTION ( 'NONE',  ( -1.000000000000000000, 0.000000000000000000, 0.000000000000000000 ) ) ;
#5543 = ORIENTED_EDGE ( 'NONE', *, *, #14941, .F. ) ;
#5544 = EDGE_CURVE ( 'NONE', #16407, #6443, #5711, .T. ) ;
#5545 = EDGE_CURVE ( 'NONE', #17341, #4393, #12084, .T. ) ;
#5546 = AXIS2_PLACEMENT_3D ( 'NONE', #12520, #6140, #16599 ) ;
#5547 = CARTESIAN_POINT ( 'NONE',  ( -90.80384757729339640, 204.6227766016838245, 0.000000000000000000 ) ) ;
#5548 = VECTOR ( 'NONE', #12877, 1000.000000000000000 ) ;
#5549 = ORIENTED_EDGE ( 'NONE', *, *, #8124, .F. ) ;
#5550 = DIRECTION ( 'NONE',  ( 0.000000000000000000, 0.000000000000000000, 1.000000000000000000 ) ) ;
#5551 =( BOUNDED_CURVE ( )  B_SPLINE_CURVE ( 3, ( #2102, #9980, #10324, #6181 ),
 .UNSPECIFIED., .F., .F. ) 
 B_SPLINE_CURVE_WITH_KNOTS ( ( 4, 4 ),
 ( 4.792629041327348460, 6.283185307179586232 ),
 .UNSPECIFIED. ) 
 CURVE ( )  GEOMETRIC_REPRESENTATION_ITEM ( )  RATIONAL_B_SPLINE_CURVE ( ( 1.000000000000000000, 0.8232662051119113977, 0.8232662051119113977, 1.000000000000000000 ) ) 
 REPRESENTATION_ITEM ( '' )  );
#5552 = ORIENTED_EDGE ( 'NONE', *, *, #5722, .F. ) ;
#5553 = CARTESIAN_POINT ( 'NONE',  ( 27.44407568426047206, 136.8394969516870958, -3.888888888888889728 ) ) ;
#5554 = DIRECTION ( 'NONE',  ( 1.000000000000000000, 0.000000000000000000, 0.000000000000000000 ) ) ;
#5555 = CARTESIAN_POINT ( 'NONE',  ( -208.0711340499744608, 166.1567726281969613, 1.827846230796970950 ) ) ;
#5556 = AXIS2_PLACEMENT_3D ( 'NONE', #16936, #6043, #7282 ) ;
#5557 = VECTOR ( 'NONE', #16924, 1000.000000000000000 ) ;
#5558 = ORIENTED_EDGE ( 'NONE', *, *, #6612, .F. ) ;
#5559 = DIRECTION ( 'NONE',  ( 0.000000000000000000, 1.000000000000000000, 0.000000000000000000 ) ) ;
#5560 = CARTESIAN_POINT ( 'NONE',  ( -95.00000000000000000, 171.6227766016838245, 25.69059892324149175 ) ) ;
#5561 = CIRCLE ( 'NONE', #16872, 2.499999999999998668 ) ;
#5562 = DIRECTION ( 'NONE',  ( 0.000000000000000000, 0.000000000000000000, -1.000000000000000000 ) ) ;
#5563 = FILL_AREA_STYLE ('',( #249 ) ) ;
#5564 = AXIS2_PLACEMENT_3D ( 'NONE', #12929, #5947, #15660 ) ;
#5565 = CARTESIAN_POINT ( 'NONE',  ( 16.31902522550215551, 136.8400131045044930, -5.103539400524613967 ) ) ;
#5566 = ORIENTED_EDGE ( 'NONE', *, *, #10985, .F. ) ;
#5567 = CARTESIAN_POINT ( 'NONE',  ( -85.00000000000002842, 146.6227766016838245, -12.99999999999999822 ) ) ;
#5568 = DIRECTION ( 'NONE',  ( 1.000000000000000000, 0.000000000000000000, 0.000000000000000000 ) ) ;
#5569 = VECTOR ( 'NONE', #5221, 1000.000000000000000 ) ;
#5570 = ORIENTED_EDGE ( 'NONE', *, *, #6017, .T. ) ;
#5571 = PRESENTATION_STYLE_ASSIGNMENT (( #9899 ) ) ;
#5572 = VECTOR ( 'NONE', #16948, 1000.000000000000000 ) ;
#5573 = CARTESIAN_POINT ( 'NONE',  ( -77.00170055202453057, 191.4074798671404949, -28.87243506922800051 ) ) ;
#5574 = DIRECTION ( 'NONE',  ( -1.000000000000000000, -0.000000000000000000, -0.000000000000000000 ) ) ;
#5575 = ADVANCED_FACE ( 'NONE', ( #5365 ), #11097, .T. ) ;
#5576 = CARTESIAN_POINT ( 'NONE',  ( 30.98806968877808998, 191.7175861903016596, 26.17636150746909607 ) ) ;
#5577 = CARTESIAN_POINT ( 'NONE',  ( 30.81698523721487604, 18.00000000000000000, -17.17210857557096659 ) ) ;
#5578 = CARTESIAN_POINT ( 'NONE',  ( -48.00000000000000000, 171.6227766016838245, 0.000000000000000000 ) ) ;
#5579 = DIRECTION ( 'NONE',  ( 1.000000000000000000, 0.000000000000000000, -0.000000000000000000 ) ) ;
#5580 = CARTESIAN_POINT ( 'NONE',  ( -7.379000772444994638, 30.00000000000000000, -25.00000000000000000 ) ) ;
#5581 = PLANE ( 'NONE',  #5807 ) ;
#5582 = ORIENTED_EDGE ( 'NONE', *, *, #10226, .T. ) ;
#5583 = DIRECTION ( 'NONE',  ( 0.000000000000000000, -0.8660254037844413721, 0.4999999999999953371 ) ) ;
#5584 = VECTOR ( 'NONE', #5200, 1000.000000000000000 ) ;
#5585 = ORIENTED_EDGE ( 'NONE', *, *, #4681, .F. ) ;
#5586 = CARTESIAN_POINT ( 'NONE',  ( -68.00000000000000000, 171.6227766016838245, 0.000000000000000000 ) ) ;
#5587 = VECTOR ( 'NONE', #7566, 1000.000000000000000 ) ;
#5588 = CARTESIAN_POINT ( 'NONE',  ( 22.50000000000001421, 146.6227766016838245, -21.54065922853802562 ) ) ;
#5589 = VERTEX_POINT ( 'NONE', #16437 ) ;
#5590 = CARTESIAN_POINT ( 'NONE',  ( -15.30535435590778448, 19.99999999999999645, 5.925683940270866756 ) ) ;
#5591 = CARTESIAN_POINT ( 'NONE',  ( -25.49999999999998579, 10.00000000000000000, 0.000000000000000000 ) ) ;
#5592 = ORIENTED_EDGE ( 'NONE', *, *, #9213, .T. ) ;
#5593 = PRODUCT ( 'Brushless DC Motor Assembly', 'Brushless DC Motor Assembly', '', ( #12343 ) ) ;
#5594 = DIRECTION ( 'NONE',  ( 0.000000000000000000, 0.000000000000000000, 1.000000000000000000 ) ) ;
#5595 = VERTEX_POINT ( 'NONE', #14913 ) ;
#5596 = EDGE_CURVE ( 'NONE', #6523, #6919, #10314, .T. ) ;
#5597 = ADVANCED_FACE ( 'NONE', ( #10921 ), #1282, .F. ) ;
#5598 = AXIS2_PLACEMENT_3D ( 'NONE', #2881, #5370, #16176 ) ;
#5599 = EDGE_CURVE ( 'NONE', #7553, #4527, #16510, .T. ) ;
#5600 = VECTOR ( 'NONE', #5746, 1000.000000000000000 ) ;
#5601 = CARTESIAN_POINT ( 'NONE',  ( -40.00000000000000000, 4.000000000000007994, 33.00000000000000711 ) ) ;
#5602 = MECHANICAL_DESIGN_GEOMETRIC_PRESENTATION_REPRESENTATION (  '', ( #5282 ), #8948 ) ;
#5603 = DIRECTION ( 'NONE',  ( -1.000000000000000000, -0.000000000000000000, 0.000000000000000000 ) ) ;
#5604 = DIRECTION ( 'NONE',  ( 1.000000000000000000, -0.000000000000000000, -0.000000000000000000 ) ) ;
#5605 = ORIENTED_EDGE ( 'NONE', *, *, #17288, .T. ) ;
#5606 = DIRECTION ( 'NONE',  ( -1.000000000000000000, 0.000000000000000000, 0.000000000000000000 ) ) ;
#5607 = ORIENTED_EDGE ( 'NONE', *, *, #14249, .T. ) ;
#5608 = DIRECTION ( 'NONE',  ( 1.000000000000000000, 0.000000000000000000, 0.000000000000000000 ) ) ;
#5609 = ORIENTED_EDGE ( 'NONE', *, *, #11549, .F. ) ;
#5610 = CARTESIAN_POINT ( 'NONE',  ( -85.45105639388464169, 191.4650750923992177, -26.36917907415269724 ) ) ;
#5611 = CARTESIAN_POINT ( 'NONE',  ( -100.0000000000000000, 144.1839557653416080, -18.33333333333335702 ) ) ;
#5612 = CARTESIAN_POINT ( 'NONE',  ( -16.30611068361787019, 32.76923076923078781, -4.999999999999999112 ) ) ;
#5613 = TOROIDAL_SURFACE ( 'NONE', #1092, 240.0000000000000000, 10.00000000000000000 ) ;
#5614 = VERTEX_POINT ( 'NONE', #16249 ) ;
#5615 = EDGE_LOOP ( 'NONE', ( #2741, #626, #3331, #6297 ) ) ;
#5616 = DIRECTION ( 'NONE',  ( -1.000000000000000000, -0.000000000000000000, 0.000000000000000000 ) ) ;
#5617 = CIRCLE ( 'NONE', #16375, 5.000000000000000888 ) ;
#5618 = CARTESIAN_POINT ( 'NONE',  ( 27.48361012698968864, 136.6227766016838245, 4.651049393634109604E-13 ) ) ;
#5619 = CARTESIAN_POINT ( 'NONE',  ( 30.00000000000000355, 196.6227766016838245, -16.00000000000000000 ) ) ;
#5620 = ORIENTED_EDGE ( 'NONE', *, *, #8168, .F. ) ;
#5621 = PRODUCT_CONTEXT ( 'NONE', #8225, 'mechanical' ) ;
#5622 = CARTESIAN_POINT ( 'NONE',  ( -45.00000000000000000, 134.2062027339443944, -25.00000000000000000 ) ) ;
#5623 = CARTESIAN_POINT ( 'NONE',  ( -70.00000000000000000, 154.3022685259950038, 9.999999999999900524 ) ) ;
#5624 = CYLINDRICAL_SURFACE ( 'NONE', #3943, 2.500000000000000444 ) ;
#5625 = DIRECTION ( 'NONE',  ( -0.000000000000000000, -0.000000000000000000, -1.000000000000000000 ) ) ;
#5626 = CARTESIAN_POINT ( 'NONE',  ( 18.50138388889793362, 17.99999999999999289, 12.24385303908842637 ) ) ;
#5627 = CIRCLE ( 'NONE', #545, 2.499999999999998668 ) ;
#5628 = CIRCLE ( 'NONE', #1381, 2.500000000000000444 ) ;
#5629 = ORIENTED_EDGE ( 'NONE', *, *, #81, .T. ) ;
#5630 = CARTESIAN_POINT ( 'NONE',  ( -81.40404063475818930, 202.4574374834314483, -16.55982638047048638 ) ) ;
#5631 = CARTESIAN_POINT ( 'NONE',  ( 1.559999999999998943, -0.8660254037844428154, 1.500000000000001332 ) ) ;
#5632 = CYLINDRICAL_SURFACE ( 'NONE', #11272, 747.9999999999998863 ) ;
#5633 = PLANE ( 'NONE',  #1671 ) ;
#5634 = DIRECTION ( 'NONE',  ( -6.938893903907228378E-16, 1.000000000000000000, 0.000000000000000000 ) ) ;
#5635 = VERTEX_POINT ( 'NONE', #4117 ) ;
#5636 = VECTOR ( 'NONE', #429, 1000.000000000000000 ) ;
#5637 = CYLINDRICAL_SURFACE ( 'NONE', #568, 5.999999999999998224 ) ;
#5638 = ADVANCED_FACE ( 'NONE', ( #6784 ), #8350, .F. ) ;
#5639 = EDGE_LOOP ( 'NONE', ( #4826, #8904 ) ) ;
#5640 = EDGE_CURVE ( 'NONE', #15415, #8582, #10057, .T. ) ;
#5641 = CARTESIAN_POINT ( 'NONE',  ( 196.0000000000000000, 175.6227766016838245, 3.071800142134975431 ) ) ;
#5642 = TOROIDAL_SURFACE ( 'NONE', #8172, -126.3651973469810628, 149.9999999999999716 ) ;
#5643 = ORIENTED_EDGE ( 'NONE', *, *, #9290, .F. ) ;
#5644 = DIRECTION ( 'NONE',  ( 1.000000000000000000, -0.000000000000000000, -0.000000000000000000 ) ) ;
#5645 = SURFACE_SIDE_STYLE ('',( #13694 ) ) ;
#5646 = CARTESIAN_POINT ( 'NONE',  ( 27.99999999999998224, 9.999999999999998224, -30.00000000000001066 ) ) ;
#5647 = ADVANCED_FACE ( 'NONE', ( #12345 ), #6864, .T. ) ;
#5648 = ORIENTED_EDGE ( 'NONE', *, *, #4820, .T. ) ;
#5649 = DIRECTION ( 'NONE',  ( 0.000000000000000000, 0.000000000000000000, 1.000000000000000000 ) ) ;
#5650 = AXIS2_PLACEMENT_3D ( 'NONE', #5819, #1491, #8292 ) ;
#5651 = DIRECTION ( 'NONE',  ( -1.000000000000000000, 0.000000000000000000, 0.000000000000000000 ) ) ;
#5652 = PLANE ( 'NONE',  #2000 ) ;
#5653 = AXIS2_PLACEMENT_3D ( 'NONE', #1210, #6532, #14317 ) ;
#5654 = DIRECTION ( 'NONE',  ( 1.000000000000000000, 0.000000000000000000, -8.673617379884036705E-17 ) ) ;
#5655 = VERTEX_POINT ( 'NONE', #5623 ) ;
#5656 = ADVANCED_FACE ( 'NONE', ( #9677 ), #16169, .F. ) ;
#5657 = PLANE ( 'NONE',  #5849 ) ;
#5658 = CARTESIAN_POINT ( 'NONE',  ( -75.00000000000000000, 196.6227766016838245, 35.00200000000000244 ) ) ;
#5659 = CIRCLE ( 'NONE', #16703, 10.00000000000000000 ) ;
#5660 = CIRCLE ( 'NONE', #11028, 20.00000000000000355 ) ;
#5661 = ORIENTED_EDGE ( 'NONE', *, *, #15270, .T. ) ;
#5662 = SURFACE_STYLE_FILL_AREA ( #1761 ) ;
#5663 = CARTESIAN_POINT ( 'NONE',  ( -81.56512917543578567, 190.8261496651129221, -29.26147795858665646 ) ) ;
#5664 = AXIS2_PLACEMENT_3D ( 'NONE', #7589, #9978, #875 ) ;
#5665 = LINE ( 'NONE', #10871, #15778 ) ;
#5666 = ADVANCED_FACE ( 'NONE', ( #2792 ), #11742, .F. ) ;
#5667 = CARTESIAN_POINT ( 'NONE',  ( 0.000000000000000000, -1.732050807568885631, 0.000000000000000000 ) ) ;
#5668 = ADVANCED_FACE ( 'NONE', ( #48 ), #15078, .T. ) ;
#5669 = DIRECTION ( 'NONE',  ( -1.000000000000000000, 0.000000000000000000, 0.000000000000000000 ) ) ;
#5670 = ADVANCED_FACE ( 'NONE', ( #4210 ), #14999, .T. ) ;
#5671 = DIRECTION ( 'NONE',  ( 1.000000000000000000, 0.000000000000000000, -0.000000000000000000 ) ) ;
#5672 = CARTESIAN_POINT ( 'NONE',  ( 19.16569565073602277, 29.91542719746881929, 11.79421528189872070 ) ) ;
#5673 = DIRECTION ( 'NONE',  ( 0.000000000000000000, 0.000000000000000000, 1.000000000000000000 ) ) ;
#5674 = SURFACE_SIDE_STYLE ('',( #16656 ) ) ;
#5675 = ORIENTED_EDGE ( 'NONE', *, *, #4065, .T. ) ;
#5676 = VERTEX_POINT ( 'NONE', #1543 ) ;
#5677 = CARTESIAN_POINT ( 'NONE',  ( 23.92105171931311958, 29.88144160311327724, -9.435928464502936208 ) ) ;
#5678 = VECTOR ( 'NONE', #8641, 1000.000000000000000 ) ;
#5679 = DIRECTION ( 'NONE',  ( -1.000000000000000000, 0.000000000000000000, 0.000000000000000000 ) ) ;
#5680 = ADVANCED_FACE ( 'NONE', ( #15345 ), #16855, .F. ) ;
#5681 = ORIENTED_EDGE ( 'NONE', *, *, #12902, .F. ) ;
#5682 = FACE_OUTER_BOUND ( 'NONE', #10377, .T. ) ;
#5683 = DIRECTION ( 'NONE',  ( 1.000000000000000000, 0.000000000000000000, -0.000000000000000000 ) ) ;
#5684 = ORIENTED_EDGE ( 'NONE', *, *, #11201, .F. ) ;
#5685 = CARTESIAN_POINT ( 'NONE',  ( 37.34717144291667523, 148.1823054118432026, -23.23525722188765741 ) ) ;
#5686 = AXIS2_PLACEMENT_3D ( 'NONE', #8874, #14617, #13296 ) ;
#5687 = CARTESIAN_POINT ( 'NONE',  ( -20.85266279178582138, 18.00000000000000000, 20.15433268689461954 ) ) ;
#5688 = CARTESIAN_POINT ( 'NONE',  ( -27.99999999999998224, 10.00000000000000000, -12.99999999999999822 ) ) ;
#5689 = PLANE ( 'NONE',  #4229 ) ;
#5690 = PLANE ( 'NONE',  #12208 ) ;
#5691 = LINE ( 'NONE', #9746, #15966 ) ;
#5692 = CARTESIAN_POINT ( 'NONE',  ( 48.00000000000000711, 163.6227766016838530, -15.00000337241049486 ) ) ;
#5693 = ORIENTED_EDGE ( 'NONE', *, *, #8827, .T. ) ;
#5694 = DIRECTION ( 'NONE',  ( 0.000000000000000000, 0.000000000000000000, -1.000000000000000000 ) ) ;
#5695 = ORIENTED_EDGE ( 'NONE', *, *, #14451, .T. ) ;
#5696 = DIRECTION ( 'NONE',  ( -0.000000000000000000, -0.000000000000000000, -1.000000000000000000 ) ) ;
#5697 = FACE_BOUND ( 'NONE', #15771, .T. ) ;
#5698 = VECTOR ( 'NONE', #3317, 1000.000000000000000 ) ;
#5699 = EDGE_CURVE ( 'NONE', #8489, #12692, #6958, .T. ) ;
#5700 = VERTEX_POINT ( 'NONE', #15521 ) ;
#5701 = ADVANCED_FACE ( 'NONE', ( #14119 ), #16775, .F. ) ;
#5702 = VERTEX_POINT ( 'NONE', #5785 ) ;
#5703 = EDGE_CURVE ( 'NONE', #1561, #3210, #1309, .T. ) ;
#5704 = EDGE_LOOP ( 'NONE', ( #11413, #4360, #17033, #8237 ) ) ;
#5705 = FACE_OUTER_BOUND ( 'NONE', #2355, .T. ) ;
#5706 = DIRECTION ( 'NONE',  ( 1.000000000000000000, 0.000000000000000000, 0.000000000000000000 ) ) ;
#5707 = CARTESIAN_POINT ( 'NONE',  ( 17.42040306417330342, 125.8667821340875577, 6.358709916038607801 ) ) ;
#5708 = ORIENTED_EDGE ( 'NONE', *, *, #10104, .F. ) ;
#5709 = CONTEXT_DEPENDENT_SHAPE_REPRESENTATION ( #2228, #8562 ) ;
#5710 = FACE_BOUND ( 'NONE', #4268, .T. ) ;
#5711 = LINE ( 'NONE', #220, #15687 ) ;
#5712 = DIRECTION ( 'NONE',  ( 1.000000000000000000, 0.000000000000000000, 0.000000000000000000 ) ) ;
#5713 = DIRECTION ( 'NONE',  ( -1.000000000000000000, 0.000000000000000000, 0.000000000000000000 ) ) ;
#5714 = CARTESIAN_POINT ( 'NONE',  ( 17.77234289100806564, 17.99999999999999289, 12.54415977683811256 ) ) ;
#5715 = ORIENTED_EDGE ( 'NONE', *, *, #8285, .F. ) ;
#5716 = FACE_OUTER_BOUND ( 'NONE', #9232, .T. ) ;
#5717 = CARTESIAN_POINT ( 'NONE',  ( -73.00000000000001421, 171.6227766016838245, 0.000000000000000000 ) ) ;
#5718 = CARTESIAN_POINT ( 'NONE',  ( 20.13757169487763576, 19.99999999999999289, -24.32197800972832624 ) ) ;
#5719 = CARTESIAN_POINT ( 'NONE',  ( 225.0000000000000000, 89.99999999999997158, 15.00000000000000000 ) ) ;
#5720 = FACE_OUTER_BOUND ( 'NONE', #6858, .T. ) ;
#5721 = VERTEX_POINT ( 'NONE', #3139 ) ;
#5722 = EDGE_CURVE ( 'NONE', #12617, #10091, #16288, .T. ) ;
#5723 = EDGE_LOOP ( 'NONE', ( #13097, #15044, #12927, #8614 ) ) ;
#5724 = DIRECTION ( 'NONE',  ( 0.000000000000000000, -1.000000000000000000, 0.000000000000000000 ) ) ;
#5725 = ORIENTED_EDGE ( 'NONE', *, *, #8449, .T. ) ;
#5726 = CARTESIAN_POINT ( 'NONE',  ( 196.0000000000000000, 167.6227766016838530, 5.571800142134975431 ) ) ;
#5727 = ORIENTED_EDGE ( 'NONE', *, *, #13749, .F. ) ;
#5728 = FACE_OUTER_BOUND ( 'NONE', #3600, .T. ) ;
#5729 = DIRECTION ( 'NONE',  ( 1.000000000000000000, 0.000000000000000000, -0.000000000000000000 ) ) ;
#5730 = ADVANCED_BREP_SHAPE_REPRESENTATION ( '', ( #11216, #3583 ), #11517 ) ;
#5731 = DIRECTION ( 'NONE',  ( -0.000000000000000000, -0.000000000000000000, -1.000000000000000000 ) ) ;
#5732 = DIRECTION ( 'NONE',  ( 0.000000000000000000, 1.734723475976807094E-15, -1.000000000000000000 ) ) ;
#5733 = EDGE_LOOP ( 'NONE', ( #7559, #1532, #5982, #2673 ) ) ;
#5734 = CARTESIAN_POINT ( 'NONE',  ( 35.00000000000000711, 146.6227766016838245, 21.54065922853802562 ) ) ;
#5735 = DIRECTION ( 'NONE',  ( 0.000000000000000000, 0.000000000000000000, -1.000000000000000000 ) ) ;
#5736 = LINE ( 'NONE', #4323, #5956 ) ;
#5737 = EDGE_CURVE ( 'NONE', #12705, #1250, #4559, .T. ) ;
#5738 = DIRECTION ( 'NONE',  ( -1.000000000000000000, -0.000000000000000000, -0.000000000000000000 ) ) ;
#5739 = PRODUCT_DEFINITION_SHAPE ( 'NONE', 'NONE',  #10297 ) ;
#5740 = CARTESIAN_POINT ( 'NONE',  ( 26.13287303778632165, 137.8093815885048627, -9.050576676228219597 ) ) ;
#5741 = ORIENTED_EDGE ( 'NONE', *, *, #3800, .F. ) ;
#5742 = FACE_BOUND ( 'NONE', #10427, .T. ) ;
#5743 = DIRECTION ( 'NONE',  ( 0.9961946980917465444, 0.08715574274764831264, 0.000000000000000000 ) ) ;
#5744 = VERTEX_POINT ( 'NONE', #8711 ) ;
#5745 = DIRECTION ( 'NONE',  ( 0.000000000000000000, 0.000000000000000000, 1.000000000000000000 ) ) ;
#5746 = DIRECTION ( 'NONE',  ( 1.000000000000000000, 0.000000000000000000, 0.000000000000000000 ) ) ;
#5747 = PLANE ( 'NONE',  #6125 ) ;
#5748 = DIRECTION ( 'NONE',  ( -1.000000000000000000, 0.000000000000000000, 0.000000000000000000 ) ) ;
#5749 = DIRECTION ( 'NONE',  ( -1.000000000000000000, 0.000000000000000000, 0.000000000000000000 ) ) ;
#5750 = CARTESIAN_POINT ( 'NONE',  ( -30.49999999999998224, 10.00000000000000000, -16.00000000000000000 ) ) ;
#5751 = CARTESIAN_POINT ( 'NONE',  ( -75.10997073956447423, 197.8146641845672491, 20.09570409464925334 ) ) ;
#5752 = EDGE_CURVE ( 'NONE', #9797, #9988, #384, .T. ) ;
#5753 = CARTESIAN_POINT ( 'NONE',  ( -24.99999999999999289, 100.0000000000000142, 0.000000000000000000 ) ) ;
#5754 = ORIENTED_EDGE ( 'NONE', *, *, #3930, .F. ) ;
#5755 = VERTEX_POINT ( 'NONE', #11364 ) ;
#5756 = CARTESIAN_POINT ( 'NONE',  ( 22.99999999999997868, 9.999999999999998224, 28.00000000000001066 ) ) ;
#5757 = DIRECTION ( 'NONE',  ( -1.000000000000000000, -0.000000000000000000, -0.000000000000000000 ) ) ;
#5758 = EDGE_LOOP ( 'NONE', ( #6654, #7465, #13604, #14997 ) ) ;
#5759 = EDGE_CURVE ( 'NONE', #1219, #6587, #11534, .T. ) ;
#5760 = DIRECTION ( 'NONE',  ( 1.000000000000000000, -0.000000000000000000, -0.000000000000000000 ) ) ;
#5761 = ADVANCED_FACE ( 'NONE', ( #7291 ), #10114, .F. ) ;
#5762 = DIRECTION ( 'NONE',  ( -1.000000000000000000, -0.000000000000000000, -0.000000000000000000 ) ) ;
#5763 = ORIENTED_EDGE ( 'NONE', *, *, #9719, .F. ) ;
#5764 = CARTESIAN_POINT ( 'NONE',  ( 24.54484354042847016, 151.7936747764227619, -26.38258506112509494 ) ) ;
#5765 = FACE_OUTER_BOUND ( 'NONE', #70, .T. ) ;
#5766 = CARTESIAN_POINT ( 'NONE',  ( 0.000000000000000000, 18.00000000000000355, 0.000000000000000000 ) ) ;
#5767 = AXIS2_PLACEMENT_3D ( 'NONE', #12788, #1991, #9862 ) ;
#5768 = FACE_OUTER_BOUND ( 'NONE', #9574, .T. ) ;
#5769 = DIRECTION ( 'NONE',  ( 1.000000000000000000, 0.000000000000000000, 0.000000000000000000 ) ) ;
#5770 = CARTESIAN_POINT ( 'NONE',  ( 34.93420767853316988, 18.00000000000000355, -4.999999999999999112 ) ) ;
#5771 = LINE ( 'NONE', #11429, #5226 ) ;
#5772 = ORIENTED_EDGE ( 'NONE', *, *, #1485, .F. ) ;
#5773 = CARTESIAN_POINT ( 'NONE',  ( -100.0000000000000000, 171.6227766016838245, 0.000000000000000000 ) ) ;
#5774 = EDGE_LOOP ( 'NONE', ( #17206, #7594, #7139, #11187, #378 ) ) ;
#5775 = CARTESIAN_POINT ( 'NONE',  ( -85.00000000000002842, 146.6227766016838245, 21.54065922853802562 ) ) ;
#5776 = ORIENTED_EDGE ( 'NONE', *, *, #1656, .F. ) ;
#5777 = ORIENTED_EDGE ( 'NONE', *, *, #8575, .T. ) ;
#5778 = ORIENTED_EDGE ( 'NONE', *, *, #2820, .F. ) ;
#5779 = CARTESIAN_POINT ( 'NONE',  ( 37.99999999999999289, 20.00000000000000000, 0.000000000000000000 ) ) ;
#5780 = VECTOR ( 'NONE', #8506, 1000.000000000000000 ) ;
#5781 = CARTESIAN_POINT ( 'NONE',  ( -5.000000000000000888, 171.6227766016838245, 0.000000000000000000 ) ) ;
#5782 = CARTESIAN_POINT ( 'NONE',  ( -31.66708739526795924, 100.0000000000000142, 5.500000000000000000 ) ) ;
#5783 = ORIENTED_EDGE ( 'NONE', *, *, #8859, .T. ) ;
#5784 = CARTESIAN_POINT ( 'NONE',  ( 40.00000000000000711, 146.6227766016838245, 0.000000000000000000 ) ) ;
#5785 = CARTESIAN_POINT ( 'NONE',  ( 37.50000000000000711, 196.6227766016838245, -13.00000000000000000 ) ) ;
#5786 = CYLINDRICAL_SURFACE ( 'NONE', #7043, 8.000000000000000000 ) ;
#5787 = FACE_OUTER_BOUND ( 'NONE', #2224, .T. ) ;
#5788 = EDGE_CURVE ( 'NONE', #16962, #243, #10902, .T. ) ;
#5789 = CARTESIAN_POINT ( 'NONE',  ( 16.74904763372935790, 29.96341334642810139, 12.79227977592015897 ) ) ;
#5790 = CYLINDRICAL_SURFACE ( 'NONE', #398, 7.499999999999996447 ) ;
#5791 = AXIS2_PLACEMENT_3D ( 'NONE', #16411, #4277, #9658 ) ;
#5792 = VERTEX_POINT ( 'NONE', #4640 ) ;
#5793 = CARTESIAN_POINT ( 'NONE',  ( -80.00000000000001421, 196.6227766016838245, 1.387778780781445676E-14 ) ) ;
#5795 = DIRECTION ( 'NONE',  ( -1.000000000000000000, -0.000000000000000000, -0.000000000000000000 ) ) ;
#5794 = AXIS2_PLACEMENT_3D ( 'NONE', #17182, #15593, #5055 ) ;
#5796 = CARTESIAN_POINT ( 'NONE',  ( 30.81698523721487604, 20.00000000000000355, -17.17210857557096659 ) ) ;
#5797 = DIRECTION ( 'NONE',  ( 1.000000000000000000, 0.000000000000000000, 0.000000000000000000 ) ) ;
#5798 = FACE_BOUND ( 'NONE', #15520, .T. ) ;
#5799 = ORIENTED_EDGE ( 'NONE', *, *, #5535, .F. ) ;
#5800 = EDGE_LOOP ( 'NONE', ( #891, #9210, #13059, #12007 ) ) ;
#5801 = CARTESIAN_POINT ( 'NONE',  ( 196.0000000000000000, 159.6227766016838814, 8.071800142134975431 ) ) ;
#5802 = ORIENTED_EDGE ( 'NONE', *, *, #240, .F. ) ;
#5803 = DIRECTION ( 'NONE',  ( -1.000000000000000000, 0.000000000000000000, 0.000000000000000000 ) ) ;
#5804 = AXIS2_PLACEMENT_3D ( 'NONE', #16366, #11036, #15020 ) ;
#5805 = ORIENTED_EDGE ( 'NONE', *, *, #12510, .F. ) ;
#5806 = LINE ( 'NONE', #8818, #5678 ) ;
#5807 = AXIS2_PLACEMENT_3D ( 'NONE', #8307, #8579, #13991 ) ;
#5808 = AXIS2_PLACEMENT_3D ( 'NONE', #13914, #6022, #16563 ) ;
#5809 = CARTESIAN_POINT ( 'NONE',  ( 196.0000000000000000, 167.6227766016838530, -3.071800142134975431 ) ) ;
#5810 = VECTOR ( 'NONE', #3690, 1000.000000000000000 ) ;
#5811 = CARTESIAN_POINT ( 'NONE',  ( -208.1430079281944074, 166.0913325906388422, 2.284806080016937635 ) ) ;
#5812 = ADVANCED_FACE ( 'NONE', ( #7123 ), #10021, .F. ) ;
#5813 = ADVANCED_FACE ( 'NONE', ( #14203 ), #8534, .T. ) ;
#5814 = CARTESIAN_POINT ( 'NONE',  ( -147.9615242270661213, 171.6227766016838245, 0.000000000000000000 ) ) ;
#5815 = EDGE_CURVE ( 'NONE', #5255, #3947, #7455, .T. ) ;
#5816 = CARTESIAN_POINT ( 'NONE',  ( 24.93034343272520204, 18.00000000000000000, -22.33460256651928333 ) ) ;
#5817 = ORIENTED_EDGE ( 'NONE', *, *, #11933, .T. ) ;
#5818 = DIRECTION ( 'NONE',  ( -0.8571673013836867971, 0.000000000000000000, -0.5150380737757237481 ) ) ;
#5819 = CARTESIAN_POINT ( 'NONE',  ( 15.00000000000000000, 171.6227766016838245, 0.000000000000000000 ) ) ;
#5820 = FACE_OUTER_BOUND ( 'NONE', #8272, .T. ) ;
#5821 = CARTESIAN_POINT ( 'NONE',  ( -40.00000000000000000, 0.000000000000000000, -30.00000000000000355 ) ) ;
#5822 = AXIS2_PLACEMENT_3D ( 'NONE', #15264, #16691, #3220 ) ;
#5823 = AXIS2_PLACEMENT_3D ( 'NONE', #231, #5634, #16520 ) ;
#5824 = DIRECTION ( 'NONE',  ( 1.000000000000000000, 0.000000000000000000, -0.000000000000000000 ) ) ;
#5825 = VERTEX_POINT ( 'NONE', #15604 ) ;
#5826 = CARTESIAN_POINT ( 'NONE',  ( -95.00000000000000000, 171.6227766016838245, -27.69059892324149530 ) ) ;
#5827 = ORIENTED_EDGE ( 'NONE', *, *, #2991, .T. ) ;
#5828 =( LENGTH_UNIT ( ) NAMED_UNIT ( * ) SI_UNIT ( .MILLI., .METRE. ) );
#5829 = CARTESIAN_POINT ( 'NONE',  ( -79.08918642097148677, 190.6879887351489060, -29.35163774059940067 ) ) ;
#5830 = EDGE_CURVE ( 'NONE', #3629, #2336, #12903, .T. ) ;
#5831 = CIRCLE ( 'NONE', #6702, 2.499999999999999556 ) ;
#5832 = CARTESIAN_POINT ( 'NONE',  ( 48.00000000000000711, 175.6227766016838245, -5.571800142134975431 ) ) ;
#5833 = CIRCLE ( 'NONE', #14034, 19.49999999999998224 ) ;
#5834 = CARTESIAN_POINT ( 'NONE',  ( -45.00000000000000000, 140.0000000000000000, -15.00000000000000000 ) ) ;
#5835 = DIRECTION ( 'NONE',  ( -1.000000000000000000, 0.000000000000000000, 0.000000000000000000 ) ) ;
#5836 = DIRECTION ( 'NONE',  ( -1.000000000000000000, 0.000000000000000000, 0.000000000000000000 ) ) ;
#5837 = DIRECTION ( 'NONE',  ( 0.000000000000000000, 0.000000000000000000, -1.000000000000000000 ) ) ;
#5838 = CARTESIAN_POINT ( 'NONE',  ( -77.05368524155726107, 200.6745000914694401, 15.65774685523815890 ) ) ;
#5839 = CARTESIAN_POINT ( 'NONE',  ( -80.00000000000002842, 146.6227766016838245, -13.00000000000000000 ) ) ;
#5840 = ORIENTED_EDGE ( 'NONE', *, *, #16909, .T. ) ;
#5841 = ORIENTED_EDGE ( 'NONE', *, *, #3394, .T. ) ;
#5842 = CARTESIAN_POINT ( 'NONE',  ( 33.66001102075547635, 19.99999999999999645, -12.05479157725600459 ) ) ;
#5843 = AXIS2_PLACEMENT_3D ( 'NONE', #16482, #2761, #8504 ) ;
#5844 = AXIS2_PLACEMENT_3D ( 'NONE', #5688, #11076, #3931 ) ;
#5845 = DIRECTION ( 'NONE',  ( -0.000000000000000000, -0.000000000000000000, -1.000000000000000000 ) ) ;
#5846 = CIRCLE ( 'NONE', #10649, 33.00000000000000000 ) ;
#5847 = ORIENTED_EDGE ( 'NONE', *, *, #15621, .F. ) ;
#5848 = CARTESIAN_POINT ( 'NONE',  ( -14.77653433949313744, 31.60550367499664759, 12.35354907637233701 ) ) ;
#5849 = AXIS2_PLACEMENT_3D ( 'NONE', #1414, #4420, #161 ) ;
#5850 = CARTESIAN_POINT ( 'NONE',  ( 225.0000000000000000, 89.99999999999997158, -15.00000000000000000 ) ) ;
#5851 = ORIENTED_EDGE ( 'NONE', *, *, #7691, .T. ) ;
#5852 = EDGE_CURVE ( 'NONE', #7172, #7959, #3404, .T. ) ;
#5853 = CARTESIAN_POINT ( 'NONE',  ( 37.25092477156690762, 148.5867852293671376, -23.63587233142070687 ) ) ;
#5854 = EDGE_CURVE ( 'NONE', #9467, #14899, #3854, .T. ) ;
#5855 = CARTESIAN_POINT ( 'NONE',  ( -32.66708739526796279, 101.0000000000000142, -4.722170599040662609 ) ) ;
#5856 = CARTESIAN_POINT ( 'NONE',  ( -45.00000000000000711, 171.6227766016838245, 0.000000000000000000 ) ) ;
#5857 = CARTESIAN_POINT ( 'NONE',  ( -207.2426727481553428, 174.8619425413479860, 4.000245852388181866 ) ) ;
#5858 = FACE_OUTER_BOUND ( 'NONE', #770, .T. ) ;
#5859 = TOROIDAL_SURFACE ( 'NONE', #8394, 40.99999999999998579, 1.000000000000000000 ) ;
#5860 = LINE ( 'NONE', #8781, #15107 ) ;
#5861 = AXIS2_PLACEMENT_3D ( 'NONE', #1106, #13327, #12975 ) ;
#5862 = ADVANCED_FACE ( 'NONE', ( #8867 ), #3744, .F. ) ;
#5863 = VECTOR ( 'NONE', #17323, 1000.000000000000000 ) ;
#5864 = DIRECTION ( 'NONE',  ( 1.000000000000000000, 0.000000000000000000, 0.000000000000000000 ) ) ;
#5865 = ORIENTED_EDGE ( 'NONE', *, *, #917, .F. ) ;
#5866 = CARTESIAN_POINT ( 'NONE',  ( 49.99999999999998579, 151.6227766016839098, 5.571800142134973655 ) ) ;
#5867 = VERTEX_POINT ( 'NONE', #1086 ) ;
#5868 = CARTESIAN_POINT ( 'NONE',  ( 39.99999999999998579, 4.000000000000007994, 33.00000000000001421 ) ) ;
#5869 = CARTESIAN_POINT ( 'NONE',  ( -14.26174088910747706, 32.16828253888332512, -10.14247415352539683 ) ) ;
#5870 = VERTEX_POINT ( 'NONE', #15683 ) ;
#5871 = CARTESIAN_POINT ( 'NONE',  ( 39.99999999999998579, 8.000000000000008882, 34.99999999999999289 ) ) ;
#5872 = AXIS2_PLACEMENT_3D ( 'NONE', #1569, #2730, #9622 ) ;
#5873 = DIRECTION ( 'NONE',  ( 0.000000000000000000, 0.000000000000000000, 1.000000000000000000 ) ) ;
#5874 = CARTESIAN_POINT ( 'NONE',  ( 15.95013150516294154, 137.1612117474554111, 8.111885438162648398 ) ) ;
#5875 = CIRCLE ( 'NONE', #10100, 2.499999999999998668 ) ;
#5876 = ORIENTED_EDGE ( 'NONE', *, *, #2212, .T. ) ;
#5877 = ITEM_DEFINED_TRANSFORMATION ( 'NONE', 'NONE', #4161,  #3583 ) ;
#5878 = CARTESIAN_POINT ( 'NONE',  ( -80.00000000000002842, 146.6227766016838245, -35.00000000000000000 ) ) ;
#5879 = CARTESIAN_POINT ( 'NONE',  ( 34.93420767853316988, 30.00000000000000000, -4.999999999999999112 ) ) ;
#5880 = CARTESIAN_POINT ( 'NONE',  ( -78.44971993548843159, 191.8535701216948155, 26.07159546787934445 ) ) ;
#5881 = CARTESIAN_POINT ( 'NONE',  ( 196.0000000000000000, 167.6227766016838530, 8.071800142134975431 ) ) ;
#5882 = CARTESIAN_POINT ( 'NONE',  ( 19.20424459521615290, 18.00000000000228439, 11.86908137778077688 ) ) ;
#5883 = PRODUCT_DEFINITION_SHAPE ( 'NONE', 'NONE',  #17532 ) ;
#5884 = DIRECTION ( 'NONE',  ( -1.000000000000000000, 0.000000000000000000, 0.000000000000000000 ) ) ;
#5885 = ADVANCED_FACE ( 'NONE', ( #14276 ), #4976, .T. ) ;
#5886 = EDGE_LOOP ( 'NONE', ( #5278, #15599, #490, #17097 ) ) ;
#5887 = LINE ( 'NONE', #7393, #3911 ) ;
#5888 = AXIS2_PLACEMENT_3D ( 'NONE', #14919, #9344, #8009 ) ;
#5889 = LINE ( 'NONE', #16698, #7380 ) ;
#5890 = VERTEX_POINT ( 'NONE', #13045 ) ;
#5891 = DIRECTION ( 'NONE',  ( 0.000000000000000000, 0.000000000000000000, -1.000000000000000000 ) ) ;
#5892 = CIRCLE ( 'NONE', #9835, 33.00000000000000000 ) ;
#5893 = DIRECTION ( 'NONE',  ( 0.000000000000000000, 0.000000000000000000, 1.000000000000000000 ) ) ;
#5894 = MECHANICAL_DESIGN_GEOMETRIC_PRESENTATION_REPRESENTATION (  '', ( #13811 ), #3627 ) ;
#5895 = ORIENTED_EDGE ( 'NONE', *, *, #2234, .F. ) ;
#5896 = VERTEX_POINT ( 'NONE', #14633 ) ;
#5897 = ORIENTED_EDGE ( 'NONE', *, *, #14197, .F. ) ;
#5898 = DIRECTION ( 'NONE',  ( 0.000000000000000000, 0.000000000000000000, 1.000000000000000000 ) ) ;
#5899 = EDGE_CURVE ( 'NONE', #2134, #13670, #1870, .T. ) ;
#5900 = ORIENTED_EDGE ( 'NONE', *, *, #2398, .T. ) ;
#5901 = DIRECTION ( 'NONE',  ( 0.000000000000000000, 0.000000000000000000, -1.000000000000000000 ) ) ;
#5902 = ORIENTED_EDGE ( 'NONE', *, *, #3800, .T. ) ;
#5903 = SURFACE_STYLE_USAGE ( .BOTH. , #12624 ) ;
#5904 = AXIS2_PLACEMENT_3D ( 'NONE', #5148, #10536, #2490 ) ;
#5905 = DIRECTION ( 'NONE',  ( 0.000000000000000000, -1.000000000000000000, 6.123233995736762338E-17 ) ) ;
#5906 = CIRCLE ( 'NONE', #12967, 12.00000000000000000 ) ;
#5907 = CARTESIAN_POINT ( 'NONE',  ( -100.0000000000000000, 199.3133755249253056, 1.695560166891042033E-15 ) ) ;
#5908 = CARTESIAN_POINT ( 'NONE',  ( 39.99999999999998579, 4.000000000000000000, -30.00000000000000000 ) ) ;
#5909 = DIRECTION ( 'NONE',  ( -0.000000000000000000, -0.000000000000000000, -1.000000000000000000 ) ) ;
#5910 = ORIENTED_EDGE ( 'NONE', *, *, #4471, .T. ) ;
#5911 = CARTESIAN_POINT ( 'NONE',  ( 29.06781294723401388, 141.7051482704754335, 13.92628470286629927 ) ) ;
#5912 = CARTESIAN_POINT ( 'NONE',  ( -153.0000000000000284, 171.6227766016838245, -6.000000000000005329 ) ) ;
#5913 = CARTESIAN_POINT ( 'NONE',  ( -95.00000000000000000, 171.6227766016838245, 0.000000000000000000 ) ) ;
#5914 = CARTESIAN_POINT ( 'NONE',  ( -8.720613081040568204, 20.00000000000000000, -24.99999999951824492 ) ) ;
#5915 = DIRECTION ( 'NONE',  ( 0.000000000000000000, 0.000000000000000000, -1.000000000000000000 ) ) ;
#5916 = AXIS2_PLACEMENT_3D ( 'NONE', #7346, #12751, #16629 ) ;
#5917 = CIRCLE ( 'NONE', #13836, 6.000000000000005329 ) ;
#5918 = VECTOR ( 'NONE', #10283, 1000.000000000000000 ) ;
#5919 = CYLINDRICAL_SURFACE ( 'NONE', #6502, 2.500000000000000444 ) ;
#5920 = EDGE_CURVE ( 'NONE', #9313, #4595, #14865, .T. ) ;
#5921 = EDGE_CURVE ( 'NONE', #5131, #8580, #13746, .T. ) ;
#5922 = EDGE_CURVE ( 'NONE', #12616, #16088, #10084, .T. ) ;
#5923 = EDGE_LOOP ( 'NONE', ( #14385, #5344, #781, #13180 ) ) ;
#5924 = CARTESIAN_POINT ( 'NONE',  ( 1.559999999999998943, -0.8660254037844428154, 1.500000000000001332 ) ) ;
#5925 = ORIENTED_EDGE ( 'NONE', *, *, #17461, .F. ) ;
#5926 = FILL_AREA_STYLE_COLOUR ( '', #6743 ) ;
#5927 = CARTESIAN_POINT ( 'NONE',  ( 23.67803828928656884, 138.9414820825090544, 12.55787835418278675 ) ) ;
#5928 = EDGE_LOOP ( 'NONE', ( #15128, #2448 ) ) ;
#5929 = CIRCLE ( 'NONE', #556, 24.99999999999999645 ) ;
#5930 = CARTESIAN_POINT ( 'NONE',  ( -43.00000000000000000, 140.0000000000000000, 0.000000000000000000 ) ) ;
#5931 = AXIS2_PLACEMENT_3D ( 'NONE', #2901, #8559, #7066 ) ;
#5932 = AXIS2_PLACEMENT_3D ( 'NONE', #645, #11085, #11433 ) ;
#5933 = LINE ( 'NONE', #10304, #11213 ) ;
#5934 = FACE_OUTER_BOUND ( 'NONE', #10749, .T. ) ;
#5935 = ORIENTED_EDGE ( 'NONE', *, *, #1819, .F. ) ;
#5936 = DIRECTION ( 'NONE',  ( -1.000000000000000000, 0.000000000000000000, 0.000000000000000000 ) ) ;
#5937 = CARTESIAN_POINT ( 'NONE',  ( 22.93524650466160963, 29.84210526315773748, 4.999999999999999112 ) ) ;
#5938 = CARTESIAN_POINT ( 'NONE',  ( -75.00000000000000000, 196.6227766016838245, 21.54065922853802206 ) ) ;
#5939 = CARTESIAN_POINT ( 'NONE',  ( 30.00000000000001066, 146.6227766016838245, -12.99999999999999822 ) ) ;
#5940 = ORIENTED_EDGE ( 'NONE', *, *, #9845, .F. ) ;
#5941 = ORIENTED_EDGE ( 'NONE', *, *, #7843, .F. ) ;
#5942 = CARTESIAN_POINT ( 'NONE',  ( 22.95484754400920124, 19.99999999999998934, -11.15425480658508306 ) ) ;
#5943 = CIRCLE ( 'NONE', #11316, 239.9999999999999716 ) ;
#5944 = CIRCLE ( 'NONE', #14417, 2.499999999999998668 ) ;
#5945 = CARTESIAN_POINT ( 'NONE',  ( 35.00000000000000000, 196.6227766016838245, 21.54065922853802206 ) ) ;
#5946 = VERTEX_POINT ( 'NONE', #17194 ) ;
#5947 = DIRECTION ( 'NONE',  ( -0.000000000000000000, -0.000000000000000000, -1.000000000000000000 ) ) ;
#5948 = AXIS2_PLACEMENT_3D ( 'NONE', #9633, #16286, #15115 ) ;
#5949 = DIRECTION ( 'NONE',  ( -0.000000000000000000, -0.000000000000000000, -1.000000000000000000 ) ) ;
#5950 = ORIENTED_EDGE ( 'NONE', *, *, #6173, .F. ) ;
#5951 = CYLINDRICAL_SURFACE ( 'NONE', #6783, 7.500000000000003553 ) ;
#5952 = CARTESIAN_POINT ( 'NONE',  ( -32.64269715136552463, 101.2195121951219647, -4.499999999999999112 ) ) ;
#5953 = CARTESIAN_POINT ( 'NONE',  ( -100.0000000000000000, 171.6227766016838245, 0.000000000000000000 ) ) ;
#5954 = DIRECTION ( 'NONE',  ( -0.000000000000000000, -0.000000000000000000, -1.000000000000000000 ) ) ;
#5955 = VECTOR ( 'NONE', #15050, 1000.000000000000000 ) ;
#5956 = VECTOR ( 'NONE', #1754, 1000.000000000000000 ) ;
#5957 = DIRECTION ( 'NONE',  ( -1.000000000000000000, 0.000000000000000000, 0.000000000000000000 ) ) ;
#5958 = DIRECTION ( 'NONE',  ( -1.000000000000000000, 0.000000000000000000, 0.000000000000000000 ) ) ;
#5959 = VECTOR ( 'NONE', #5905, 1000.000000000000000 ) ;
#5960 = CARTESIAN_POINT ( 'NONE',  ( -208.3486229709906468, 178.7173894086183168, 0.000000000000000000 ) ) ;
#5961 = EDGE_LOOP ( 'NONE', ( #8883, #3624, #6841, #7009 ) ) ;
#5962 = DIRECTION ( 'NONE',  ( 1.000000000000000000, 0.000000000000000000, 0.000000000000000000 ) ) ;
#5963 = ORIENTED_EDGE ( 'NONE', *, *, #12607, .T. ) ;
#5964 = EDGE_CURVE ( 'NONE', #8896, #160, #8367, .T. ) ;
#5965 = DIRECTION ( 'NONE',  ( 0.000000000000000000, 2.775557561562891351E-15, 1.000000000000000000 ) ) ;
#5966 = CARTESIAN_POINT ( 'NONE',  ( -25.81010901361623056, 18.00000000000000000, -13.97188021846430139 ) ) ;
#5967 = ORIENTED_EDGE ( 'NONE', *, *, #11776, .F. ) ;
#5968 = CARTESIAN_POINT ( 'NONE',  ( -151.0000000000000284, 171.6227766016838245, -23.57392898041431195 ) ) ;
#5969 = CIRCLE ( 'NONE', #9912, 249.9999999999999716 ) ;
#5970 = LINE ( 'NONE', #16685, #9309 ) ;
#5971 = CARTESIAN_POINT ( 'NONE',  ( 16.24385689529520604, 136.8350826111700655, 4.682368943704262598 ) ) ;
#5972 = ORIENTED_EDGE ( 'NONE', *, *, #7869, .T. ) ;
#5973 = FACE_OUTER_BOUND ( 'NONE', #1810, .T. ) ;
#5974 = DIRECTION ( 'NONE',  ( -0.000000000000000000, -0.000000000000000000, -1.000000000000000000 ) ) ;
#5975 = CYLINDRICAL_SURFACE ( 'NONE', #7896, 2.500000000000000444 ) ;
#5976 = LINE ( 'NONE', #11366, #7657 ) ;
#5977 = CARTESIAN_POINT ( 'NONE',  ( 17.00458606767794834, 29.95830270928036398, 12.72829919683579902 ) ) ;
#5978 = DIRECTION ( 'NONE',  ( 0.000000000000000000, 0.000000000000000000, 1.000000000000000000 ) ) ;
#5979 = ORIENTED_EDGE ( 'NONE', *, *, #1438, .T. ) ;
#5980 = CARTESIAN_POINT ( 'NONE',  ( -32.59761674097720174, 100.6207349242430809, 5.080178642862614780 ) ) ;
#5981 = DIRECTION ( 'NONE',  ( -1.000000000000000000, 0.000000000000000000, 0.000000000000000000 ) ) ;
#5982 = ORIENTED_EDGE ( 'NONE', *, *, #9588, .T. ) ;
#5983 = EDGE_CURVE ( 'NONE', #15728, #7056, #11621, .T. ) ;
#5984 = DIRECTION ( 'NONE',  ( -1.000000000000000000, 0.000000000000000000, 0.000000000000000000 ) ) ;
#5985 = FACE_OUTER_BOUND ( 'NONE', #10484, .T. ) ;
#5986 = ORIENTED_EDGE ( 'NONE', *, *, #9161, .F. ) ;
#5987 = ORIENTED_EDGE ( 'NONE', *, *, #10951, .T. ) ;
#5988 = ADVANCED_FACE ( 'NONE', ( #10281 ), #8960, .T. ) ;
#5989 = CARTESIAN_POINT ( 'NONE',  ( 10.09659264799822331, 132.0789811519323962, 12.16719622200489681 ) ) ;
#5990 = ORIENTED_EDGE ( 'NONE', *, *, #12095, .T. ) ;
#5991 = EDGE_CURVE ( 'NONE', #17383, #134, #15147, .T. ) ;
#5992 = CARTESIAN_POINT ( 'NONE',  ( 30.00000000000000355, 196.6227766016838245, -12.99999999999999822 ) ) ;
#5993 = ADVANCED_FACE ( 'NONE', ( #5069 ), #16581, .T. ) ;
#5994 = ORIENTED_EDGE ( 'NONE', *, *, #7134, .T. ) ;
#5995 = LINE ( 'NONE', #8733, #9901 ) ;
#5996 = FILL_AREA_STYLE_COLOUR ( '', #15135 ) ;
#5997 = DIRECTION ( 'NONE',  ( -1.000000000000000000, -0.000000000000000000, -0.000000000000000000 ) ) ;
#5998 = CYLINDRICAL_SURFACE ( 'NONE', #9477, 7.500000000000003553 ) ;
#5999 = ORIENTED_EDGE ( 'NONE', *, *, #12413, .T. ) ;
#6000 = CARTESIAN_POINT ( 'NONE',  ( 31.71694765202421351, 141.9230918234059402, 14.38591257614910823 ) ) ;
#6001 = DIRECTION ( 'NONE',  ( 0.000000000000000000, 0.000000000000000000, 1.000000000000000000 ) ) ;
#6002 = DIRECTION ( 'NONE',  ( 1.000000000000000000, 0.000000000000000000, 0.000000000000000000 ) ) ;
#6003 = CARTESIAN_POINT ( 'NONE',  ( -13.66886994730069560, 31.37497952739824214, -13.17845503416513075 ) ) ;
#6004 = CARTESIAN_POINT ( 'NONE',  ( -22.99999999999998224, 10.00000000000000000, 0.000000000000000000 ) ) ;
#6005 = DIRECTION ( 'NONE',  ( -1.000000000000000000, 0.000000000000000000, 0.000000000000000000 ) ) ;
#6006 = VERTEX_POINT ( 'NONE', #7901 ) ;
#6007 = CARTESIAN_POINT ( 'NONE',  ( 49.99999999999998579, 187.6227766016837961, -15.00000337241049486 ) ) ;
#6008 = EDGE_LOOP ( 'NONE', ( #7802, #11194, #4243, #8727 ) ) ;
#6009 =( LENGTH_UNIT ( ) NAMED_UNIT ( * ) SI_UNIT ( .MILLI., .METRE. ) );
#6010 = CARTESIAN_POINT ( 'NONE',  ( -85.72866685541674769, 194.8302331505971949, -26.20043099198422354 ) ) ;
#6011 = CARTESIAN_POINT ( 'NONE',  ( -80.00000000000001421, 196.6227766016838245, -35.00000000000000000 ) ) ;
#6012 = LINE ( 'NONE', #4684, #13405 ) ;
#6013 = EDGE_LOOP ( 'NONE', ( #16866, #9174, #3361, #11111 ) ) ;
#6014 = FACE_OUTER_BOUND ( 'NONE', #10183, .T. ) ;
#6015 = DIRECTION ( 'NONE',  ( -1.000000000000000000, 0.000000000000000000, 0.000000000000000000 ) ) ;
#6016 = ADVANCED_FACE ( 'NONE', ( #6226 ), #14457, .T. ) ;
#6017 = EDGE_CURVE ( 'NONE', #11430, #3475, #601, .T. ) ;
#6018 = CARTESIAN_POINT ( 'NONE',  ( -75.82181986242348160, 199.3841150854655666, 17.84683500849085647 ) ) ;
#6019 = EDGE_CURVE ( 'NONE', #15920, #14931, #13470, .T. ) ;
#6020 = ORIENTED_EDGE ( 'NONE', *, *, #2781, .T. ) ;
#6021 = ORIENTED_EDGE ( 'NONE', *, *, #6191, .F. ) ;
#6022 = DIRECTION ( 'NONE',  ( -1.000000000000000000, -0.000000000000000000, -0.000000000000000000 ) ) ;
#6023 = CARTESIAN_POINT ( 'NONE',  ( 49.99999999999998579, 159.6227766016838814, 3.071800142134975431 ) ) ;
#6024 = ORIENTED_EDGE ( 'NONE', *, *, #2073, .F. ) ;
#6025 = FACE_OUTER_BOUND ( 'NONE', #4859, .T. ) ;
#6026 = LINE ( 'NONE', #10089, #10162 ) ;
#6027 = ORIENTED_EDGE ( 'NONE', *, *, #8887, .T. ) ;
#6028 = FACE_BOUND ( 'NONE', #9614, .T. ) ;
#6029 = CARTESIAN_POINT ( 'NONE',  ( -14.99999999999998579, 90.00000000000000000, 4.999999999999999112 ) ) ;
#6030 = DIRECTION ( 'NONE',  ( 0.000000000000000000, 0.000000000000000000, -1.000000000000000000 ) ) ;
#6031 = LINE ( 'NONE', #10000, #15406 ) ;
#6032 = CARTESIAN_POINT ( 'NONE',  ( -16.41264213764166513, 18.00000000000000000, 23.02790928165778794 ) ) ;
#6033 = ADVANCED_FACE ( 'NONE', ( #989 ), #3834, .T. ) ;
#6034 = ADVANCED_FACE ( 'NONE', ( #1613 ), #1026, .F. ) ;
#6035 = CARTESIAN_POINT ( 'NONE',  ( -77.50000000000002842, 146.6227766016838245, -16.00000000000000000 ) ) ;
#6036 = ADVANCED_FACE ( 'NONE', ( #16230 ), #1356, .F. ) ;
#6037 = EDGE_CURVE ( 'NONE', #8060, #4330, #8379, .T. ) ;
#6038 = DIRECTION ( 'NONE',  ( -1.000000000000000000, 0.000000000000000000, 0.000000000000000000 ) ) ;
#6039 = EDGE_LOOP ( 'NONE', ( #5149, #6252, #16658, #4787 ) ) ;
#6040 = PLANE ( 'NONE',  #13243 ) ;
#6041 = ORIENTED_EDGE ( 'NONE', *, *, #2079, .F. ) ;
#6042 = CARTESIAN_POINT ( 'NONE',  ( 22.99999999999997868, 9.999999999999998224, 35.00200000000000244 ) ) ;
#6043 = DIRECTION ( 'NONE',  ( -0.000000000000000000, -0.000000000000000000, 1.000000000000000000 ) ) ;
#6044 = ORIENTED_EDGE ( 'NONE', *, *, #13788, .T. ) ;
#6045 = DIRECTION ( 'NONE',  ( 0.000000000000000000, 0.000000000000000000, 1.000000000000000000 ) ) ;
#6046 = CARTESIAN_POINT ( 'NONE',  ( 24.41196201396447663, 20.00000000000113687, 8.570466955472159754 ) ) ;
#6047 = CARTESIAN_POINT ( 'NONE',  ( 27.44407568426053246, 136.8394969516870958, 3.888888888888893725 ) ) ;
#6048 = ORIENTED_EDGE ( 'NONE', *, *, #337, .T. ) ;
#6049 = FACE_OUTER_BOUND ( 'NONE', #13049, .T. ) ;
#6050 = ADVANCED_FACE ( 'NONE', ( #1446 ), #8161, .T. ) ;
#6051 = CARTESIAN_POINT ( 'NONE',  ( 17.00000000000000000, 171.6227766016838245, 0.000000000000000000 ) ) ;
#6052 = CARTESIAN_POINT ( 'NONE',  ( -80.77514562707608547, 191.6792914357319262, 26.20566807848922863 ) ) ;
#6053 = CARTESIAN_POINT ( 'NONE',  ( 1.559999999999998943, 0.000000000000000000, 1.500000000000001332 ) ) ;
#6054 = FACE_OUTER_BOUND ( 'NONE', #11289, .T. ) ;
#6055 = FACE_OUTER_BOUND ( 'NONE', #11656, .T. ) ;
#6056 = ORIENTED_EDGE ( 'NONE', *, *, #17198, .F. ) ;
#6057 = DIRECTION ( 'NONE',  ( -0.000000000000000000, -0.000000000000000000, -1.000000000000000000 ) ) ;
#6058 = CARTESIAN_POINT ( 'NONE',  ( 39.99999999999998579, 0.000000000000000000, 33.00000000000000711 ) ) ;
#6059 = ORIENTED_EDGE ( 'NONE', *, *, #15800, .F. ) ;
#6060 = DIRECTION ( 'NONE',  ( 0.000000000000000000, -0.4999999999999952816, 0.8660254037844413721 ) ) ;
#6061 = CARTESIAN_POINT ( 'NONE',  ( -22.93725393319379791, 120.0000000000000284, 6.000000000000001776 ) ) ;
#6062 = AXIS2_PLACEMENT_3D ( 'NONE', #14280, #15610, #2152 ) ;
#6063 = ORIENTED_EDGE ( 'NONE', *, *, #12794, .F. ) ;
#6064 = AXIS2_PLACEMENT_3D ( 'NONE', #14759, #12005, #15072 ) ;
#6065 = ORIENTED_EDGE ( 'NONE', *, *, #1642, .F. ) ;
#6066 = VERTEX_POINT ( 'NONE', #284 ) ;
#6067 = ORIENTED_EDGE ( 'NONE', *, *, #11396, .F. ) ;
#6068 = DIRECTION ( 'NONE',  ( 0.000000000000000000, 0.000000000000000000, 1.000000000000000000 ) ) ;
#6069 = ORIENTED_EDGE ( 'NONE', *, *, #11935, .T. ) ;
#6070 = FACE_OUTER_BOUND ( 'NONE', #3696, .T. ) ;
#6071 = EDGE_CURVE ( 'NONE', #3416, #9987, #13480, .T. ) ;
#6072 = CARTESIAN_POINT ( 'NONE',  ( -75.00000000000000000, 196.6227766016838245, 0.000000000000000000 ) ) ;
#6073 = VECTOR ( 'NONE', #6119, 1000.000000000000000 ) ;
#6074 = CARTESIAN_POINT ( 'NONE',  ( -25.49999999999998579, 10.00000000000000000, 10.00000000000000178 ) ) ;
#6075 = DIRECTION ( 'NONE',  ( 0.000000000000000000, 0.000000000000000000, 1.000000000000000000 ) ) ;
#6076 = CIRCLE ( 'NONE', #2390, 20.00000000000000355 ) ;
#6077 = ORIENTED_EDGE ( 'NONE', *, *, #8189, .F. ) ;
#6078 = CARTESIAN_POINT ( 'NONE',  ( 35.00000000000000711, 146.3163998792643667, 21.18507967179266416 ) ) ;
#6079 = DIRECTION ( 'NONE',  ( 1.000000000000000000, 0.000000000000000000, 0.000000000000000000 ) ) ;
#6080 = EDGE_CURVE ( 'NONE', #16562, #7137, #5831, .T. ) ;
#6081 = CARTESIAN_POINT ( 'NONE',  ( -13.91527097789397160, 19.99999999999999645, -23.98152295253190758 ) ) ;
#6082 = DIRECTION ( 'NONE',  ( 0.000000000000000000, 0.000000000000000000, 1.000000000000000000 ) ) ;
#6083 = EDGE_CURVE ( 'NONE', #6776, #925, #105, .T. ) ;
#6084 = VECTOR ( 'NONE', #11950, 1000.000000000000114 ) ;
#6085 = DIRECTION ( 'NONE',  ( 0.000000000000000000, 0.000000000000000000, -1.000000000000000000 ) ) ;
#6086 = VECTOR ( 'NONE', #17251, 1000.000000000000000 ) ;
#6087 = ORIENTED_EDGE ( 'NONE', *, *, #2303, .T. ) ;
#6088 = DIRECTION ( 'NONE',  ( 0.000000000000000000, 1.000000000000000000, 0.000000000000000000 ) ) ;
#6089 = VECTOR ( 'NONE', #10231, 1000.000000000000000 ) ;
#6090 = EDGE_LOOP ( 'NONE', ( #14275, #13033, #4314, #2729 ) ) ;
#6091 = CARTESIAN_POINT ( 'NONE',  ( 19.49215236471922807, 140.4173771131980857, 15.85404464849102268 ) ) ;
#6092 = FACE_OUTER_BOUND ( 'NONE', #13347, .T. ) ;
#6093 = CARTESIAN_POINT ( 'NONE',  ( 12.84413890157916782, 129.3215245152910313, -10.42375118840982573 ) ) ;
#6094 = PRODUCT_RELATED_PRODUCT_CATEGORY ( 'part', '', ( #15498 ) ) ;
#6095 = VECTOR ( 'NONE', #7828, 1000.000000000000000 ) ;
#6096 = VERTEX_POINT ( 'NONE', #5340 ) ;
#6097 = LINE ( 'NONE', #4861, #15523 ) ;
#6098 = VECTOR ( 'NONE', #9428, 1000.000000000000000 ) ;
#6099 = CARTESIAN_POINT ( 'NONE',  ( -75.53359938325087342, 198.8884873102157940, 18.59522663992144231 ) ) ;
#6100 = EDGE_CURVE ( 'NONE', #12567, #7725, #6916, .T. ) ;
#6101 = ORIENTED_EDGE ( 'NONE', *, *, #176, .F. ) ;
#6102 = CIRCLE ( 'NONE', #737, 10.00000000000000178 ) ;
#6103 = ORIENTED_EDGE ( 'NONE', *, *, #16073, .T. ) ;
#6104 = CARTESIAN_POINT ( 'NONE',  ( 23.77503517897789465, 19.99999999999999645, -22.95135521423388170 ) ) ;
#6105 = CARTESIAN_POINT ( 'NONE',  ( -3.000000000000002665, 142.8100939375178200, -16.63501009223129756 ) ) ;
#6106 = ORIENTED_EDGE ( 'NONE', *, *, #11641, .F. ) ;
#6107 = DIRECTION ( 'NONE',  ( 0.000000000000000000, 0.000000000000000000, -1.000000000000000000 ) ) ;
#6108 = CIRCLE ( 'NONE', #743, 108.0000000000000142 ) ;
#6109 = DIRECTION ( 'NONE',  ( -1.000000000000000000, -0.000000000000000000, -0.000000000000000000 ) ) ;
#6110 = AXIS2_PLACEMENT_3D ( 'NONE', #1638, #9418, #1377 ) ;
#6111 = ORIENTED_EDGE ( 'NONE', *, *, #8449, .F. ) ;
#6112 = EDGE_CURVE ( 'NONE', #5181, #10830, #10736, .T. ) ;
#6113 = VECTOR ( 'NONE', #10748, 1000.000000000000000 ) ;
#6114 = FACE_OUTER_BOUND ( 'NONE', #5639, .T. ) ;
#6115 = UNCERTAINTY_MEASURE_WITH_UNIT (LENGTH_MEASURE( 1.000000000000000082E-05 ), #1398, 'distance_accuracy_value', 'NONE');
#6116 = CARTESIAN_POINT ( 'NONE',  ( 1.559999999999998943, -1.732050807568885631, 0.000000000000000000 ) ) ;
#6117 = DIRECTION ( 'NONE',  ( 1.000000000000000000, 0.000000000000000000, -0.000000000000000000 ) ) ;
#6118 = CARTESIAN_POINT ( 'NONE',  ( -16.30611068361414695, 32.76923076921517008, 5.528684565802741702 ) ) ;
#6119 = DIRECTION ( 'NONE',  ( 0.000000000000000000, -1.000000000000000000, 0.000000000000000000 ) ) ;
#6120 = CIRCLE ( 'NONE', #758, 35.00000000000000000 ) ;
#6121 = CARTESIAN_POINT ( 'NONE',  ( -95.00000000000000000, 141.6227766016838245, 5.510910596163088767E-15 ) ) ;
#6122 = VECTOR ( 'NONE', #29, 1000.000000000000000 ) ;
#6123 = ORIENTED_EDGE ( 'NONE', *, *, #1226, .T. ) ;
#6124 = DIRECTION ( 'NONE',  ( 0.000000000000000000, -0.4999999999999996114, -0.8660254037844388186 ) ) ;
#6125 = AXIS2_PLACEMENT_3D ( 'NONE', #12216, #13906, #1423 ) ;
#6126 = ORIENTED_EDGE ( 'NONE', *, *, #7865, .F. ) ;
#6127 = DIRECTION ( 'NONE',  ( -1.000000000000000000, -0.000000000000000000, 0.000000000000000000 ) ) ;
#6128 = VECTOR ( 'NONE', #10343, 1000.000000000000000 ) ;
#6129 = CARTESIAN_POINT ( 'NONE',  ( -151.0000000000000284, 171.6227766016838245, -23.57392898041429774 ) ) ;
#6130 = ORIENTED_EDGE ( 'NONE', *, *, #10104, .T. ) ;
#6131 = CARTESIAN_POINT ( 'NONE',  ( 28.15871609335591685, 19.99999999999999289, 20.05978710182010971 ) ) ;
#6132 = EDGE_CURVE ( 'NONE', #16282, #14332, #10897, .T. ) ;
#6133 = EDGE_CURVE ( 'NONE', #8547, #6832, #2854, .T. ) ;
#6134 = CARTESIAN_POINT ( 'NONE',  ( 23.18512258076559007, 19.99999999999999645, 23.22991426836919260 ) ) ;
#6135 = EDGE_CURVE ( 'NONE', #2717, #1481, #9571, .T. ) ;
#6136 = CARTESIAN_POINT ( 'NONE',  ( 49.99999999999998579, 175.6227766016838530, 19.42820660268601074 ) ) ;
#6137 = ORIENTED_EDGE ( 'NONE', *, *, #5699, .T. ) ;
#6138 = CIRCLE ( 'NONE', #12647, 12.00000000000000000 ) ;
#6139 = AXIS2_PLACEMENT_3D ( 'NONE', #14391, #2526, #10299 ) ;
#6140 = DIRECTION ( 'NONE',  ( 0.000000000000000000, -0.000000000000000000, -1.000000000000000000 ) ) ;
#6141 = DIRECTION ( 'NONE',  ( 0.000000000000000000, 0.000000000000000000, 1.000000000000000000 ) ) ;
#6142 = LINE ( 'NONE', #17472, #15017 ) ;
#6143 = CARTESIAN_POINT ( 'NONE',  ( 196.0000000000000000, 167.6227766016838814, 19.42820660268601074 ) ) ;
#6144 = CARTESIAN_POINT ( 'NONE',  ( -40.00000000000000000, 20.00000000000000000, 0.000000000000000000 ) ) ;
#6145 = VERTEX_POINT ( 'NONE', #13655 ) ;
#6146 = DIRECTION ( 'NONE',  ( -1.000000000000000000, 0.000000000000000000, 0.000000000000000000 ) ) ;
#6147 = CARTESIAN_POINT ( 'NONE',  ( -77.50000000000002842, 146.6227766016838245, 10.00000000000000178 ) ) ;
#6148 = EDGE_LOOP ( 'NONE', ( #16961, #14090, #16502, #6908 ) ) ;
#6149 = CARTESIAN_POINT ( 'NONE',  ( 24.02486036880400277, 195.9845216101234939, -25.13379275193915063 ) ) ;
#6150 = DIRECTION ( 'NONE',  ( 1.000000000000000000, 0.000000000000000000, -0.000000000000000000 ) ) ;
#6151 = VECTOR ( 'NONE', #1144, 1000.000000000000000 ) ;
#6152 = ORIENTED_EDGE ( 'NONE', *, *, #7734, .T. ) ;
#6153 = CIRCLE ( 'NONE', #2472, 25.69059892324149175 ) ;
#6154 = ORIENTED_EDGE ( 'NONE', *, *, #12145, .F. ) ;
#6155 = ORIENTED_EDGE ( 'NONE', *, *, #4526, .F. ) ;
#6156 = VECTOR ( 'NONE', #5085, 1000.000000000000000 ) ;
#6157 = ORIENTED_EDGE ( 'NONE', *, *, #9081, .F. ) ;
#6158 = FACE_OUTER_BOUND ( 'NONE', #2536, .T. ) ;
#6159 = EDGE_CURVE ( 'NONE', #14798, #16088, #1520, .T. ) ;
#6160 = ORIENTED_EDGE ( 'NONE', *, *, #10501, .F. ) ;
#6161 =( NAMED_UNIT ( * ) PLANE_ANGLE_UNIT ( ) SI_UNIT ( $, .RADIAN. ) );
#6162 = DIRECTION ( 'NONE',  ( 0.9961946980917461003, -0.04357787137382628656, 0.07547908730516766918 ) ) ;
#6163 = CARTESIAN_POINT ( 'NONE',  ( 6.134011831684049731, 134.2062027339443944, 13.00000000000000000 ) ) ;
#6164 = CARTESIAN_POINT ( 'NONE',  ( -100.0000000000000000, 142.8100939375178200, 16.63501009223129756 ) ) ;
#6165 = AXIS2_PLACEMENT_3D ( 'NONE', #11721, #5008, #17131 ) ;
#6166 = CIRCLE ( 'NONE', #3055, 2.500000000000002220 ) ;
#6167 = ORIENTED_EDGE ( 'NONE', *, *, #572, .F. ) ;
#6168 = CARTESIAN_POINT ( 'NONE',  ( 25.63134405897505985, 139.9845197017440057, 9.403501633128708903 ) ) ;
#6169 = DIRECTION ( 'NONE',  ( 1.000000000000000000, 0.000000000000000000, 0.000000000000000000 ) ) ;
#6170 = CARTESIAN_POINT ( 'NONE',  ( -40.00000000000000000, 20.00000000000000000, -30.00000000000000355 ) ) ;
#6171 = CARTESIAN_POINT ( 'NONE',  ( -24.81085081035532269, 19.99999999999999645, -15.69149817756037457 ) ) ;
#6172 =( NAMED_UNIT ( * ) PLANE_ANGLE_UNIT ( ) SI_UNIT ( $, .RADIAN. ) );
#6173 = EDGE_CURVE ( 'NONE', #6571, #4289, #12319, .T. ) ;
#6174 = DIRECTION ( 'NONE',  ( -1.000000000000000000, -0.000000000000000000, -0.000000000000000000 ) ) ;
#6175 = VECTOR ( 'NONE', #13034, 1000.000000000000000 ) ;
#6176 = VERTEX_POINT ( 'NONE', #4276 ) ;
#6177 = CARTESIAN_POINT ( 'NONE',  ( -95.00000000000000000, 171.6227766016838245, 0.000000000000000000 ) ) ;
#6178 = VECTOR ( 'NONE', #8753, 1000.000000000000000 ) ;
#6179 = ORIENTED_EDGE ( 'NONE', *, *, #1328, .F. ) ;
#6180 = CARTESIAN_POINT ( 'NONE',  ( 39.99999999999998579, -20.00000000000000000, 34.99999999999999289 ) ) ;
#6181 = CARTESIAN_POINT ( 'NONE',  ( -187.6513770290094385, 171.1853623553244006, 0.7576236986490064718 ) ) ;
#6182 = DIRECTION ( 'NONE',  ( -0.08715574274764831264, -0.4980973490458652231, -0.8627299156628261967 ) ) ;
#6183 = EDGE_LOOP ( 'NONE', ( #17030, #16710, #7087, #1508 ) ) ;
#6184 = LINE ( 'NONE', #11584, #1343 ) ;
#6185 = CARTESIAN_POINT ( 'NONE',  ( -20.00000000000000355, 171.6227766016838245, 0.000000000000000000 ) ) ;
#6186 = AXIS2_PLACEMENT_3D ( 'NONE', #15789, #9059, #2157 ) ;
#6187 = DIRECTION ( 'NONE',  ( 0.000000000000000000, 0.000000000000000000, 1.000000000000000000 ) ) ;
#6188 = DIRECTION ( 'NONE',  ( -0.000000000000000000, 1.000000000000000000, 0.000000000000000000 ) ) ;
#6189 = VERTEX_POINT ( 'NONE', #12414 ) ;
#6190 = ORIENTED_EDGE ( 'NONE', *, *, #13391, .F. ) ;
#6191 = EDGE_CURVE ( 'NONE', #7175, #8522, #1881, .T. ) ;
#6192 = CARTESIAN_POINT ( 'NONE',  ( 20.42763382733002686, 19.99999999999999645, -24.23318166603087676 ) ) ;
#6193 = B_SPLINE_CURVE_WITH_KNOTS ( 'NONE', 3,
 ( #3302, #14111, #4718, #10107, #15598, #14360, #12685, #562, #5966, #10009, #15512, #11780, #6381, #15946, #3821, #13471, #13381, #14450, #5061, #4968, #9123, #11874, #13116, #11961, #8059, #10539 ),
 .UNSPECIFIED., .F., .F.,
 ( 4, 2, 2, 2, 2, 2, 2, 2, 2, 2, 2, 2, 4 ),
 ( 0.000000000000000000, 0.002002783134349999609, 0.004005566268699999218, 0.008011132537399998435, 0.01001391567174999414, 0.01201669880609998985, 0.01602226507479997952, 0.01802504820914997002, 0.02002783134349995706, 0.02403339761219993806, 0.02603618074654992856, 0.02803896388089991906, 0.03204453014959990353 ),
 .UNSPECIFIED. ) ;
#6194 = CARTESIAN_POINT ( 'NONE',  ( -30.49999999999998224, 10.00000000000000000, 10.00000000000000178 ) ) ;
#6195 = VERTEX_POINT ( 'NONE', #7987 ) ;
#6196 = DIRECTION ( 'NONE',  ( 0.000000000000000000, 0.000000000000000000, -1.000000000000000000 ) ) ;
#6197 = CARTESIAN_POINT ( 'NONE',  ( 7.010070850707991852, 140.5745599005093709, -12.93128425348633570 ) ) ;
#6198 = VECTOR ( 'NONE', #772, 1000.000000000000000 ) ;
#6199 = EDGE_CURVE ( 'NONE', #5097, #793, #13392, .T. ) ;
#6200 = ORIENTED_EDGE ( 'NONE', *, *, #2879, .T. ) ;
#6201 = CIRCLE ( 'NONE', #12717, 2.500000000000002220 ) ;
#6202 = DIRECTION ( 'NONE',  ( -0.000000000000000000, -1.000000000000000000, -0.000000000000000000 ) ) ;
#6203 = ADVANCED_FACE ( 'NONE', ( #9401 ), #14805, .T. ) ;
#6204 = AXIS2_PLACEMENT_3D ( 'NONE', #6575, #17368, #2406 ) ;
#6205 = ADVANCED_FACE ( 'NONE', ( #3288 ), #4353, .T. ) ;
#6206 = CARTESIAN_POINT ( 'NONE',  ( 30.00000000000000355, 196.6227766016838245, 0.000000000000000000 ) ) ;
#6207 = CARTESIAN_POINT ( 'NONE',  ( 34.93420767853318409, 18.00000000000000000, -5.000000000000010658 ) ) ;
#6208 = CARTESIAN_POINT ( 'NONE',  ( -14.07899634757819385, 32.11373924370096233, 10.33209047619764753 ) ) ;
#6209 = CARTESIAN_POINT ( 'NONE',  ( 196.0000000000000000, 187.6227766016837961, -12.50000337241049309 ) ) ;
#6210 = FACE_OUTER_BOUND ( 'NONE', #377, .T. ) ;
#6211 = EDGE_LOOP ( 'NONE', ( #13976, #2774, #3893, #14071 ) ) ;
#6212 = DIRECTION ( 'NONE',  ( -1.000000000000000000, -0.000000000000000000, -0.000000000000000000 ) ) ;
#6213 = CIRCLE ( 'NONE', #569, 10.00000000000000000 ) ;
#6214 = ADVANCED_FACE ( 'NONE', ( #15328 ), #16019, .F. ) ;
#6215 = ORIENTED_EDGE ( 'NONE', *, *, #10468, .T. ) ;
#6216 = DIRECTION ( 'NONE',  ( -0.000000000000000000, -0.000000000000000000, -1.000000000000000000 ) ) ;
#6217 = AXIS2_PLACEMENT_3D ( 'NONE', #16383, #4423, #12214 ) ;
#6218 = FACE_BOUND ( 'NONE', #16873, .T. ) ;
#6219 = ORIENTED_EDGE ( 'NONE', *, *, #4895, .T. ) ;
#6220 = LINE ( 'NONE', #1888, #13124 ) ;
#6221 = CARTESIAN_POINT ( 'NONE',  ( 22.30340133326367180, 20.00000000000000000, 11.90876978475634651 ) ) ;
#6222 = VECTOR ( 'NONE', #9785, 1000.000000000000000 ) ;
#6223 = VECTOR ( 'NONE', #15296, 1000.000000000000000 ) ;
#6224 = VERTEX_POINT ( 'NONE', #4623 ) ;
#6225 = AXIS2_PLACEMENT_3D ( 'NONE', #13596, #4296, #8182 ) ;
#6226 = FACE_OUTER_BOUND ( 'NONE', #7354, .T. ) ;
#6227 = CARTESIAN_POINT ( 'NONE',  ( -68.00000000000000000, 171.6227766016838245, 19.49999999999999645 ) ) ;
#6228 = CARTESIAN_POINT ( 'NONE',  ( -16.47274440071381107, 31.95215739789422571, -10.50982007662407725 ) ) ;
#6229 = LINE ( 'NONE', #7204, #2097 ) ;
#6230 = VERTEX_POINT ( 'NONE', #1961 ) ;
#6231 = FACE_OUTER_BOUND ( 'NONE', #1167, .T. ) ;
#6232 = EDGE_CURVE ( 'NONE', #216, #4054, #9998, .T. ) ;
#6233 = EDGE_CURVE ( 'NONE', #17520, #6671, #9499, .T. ) ;
#6234 = DIRECTION ( 'NONE',  ( 0.000000000000000000, 0.000000000000000000, 1.000000000000000000 ) ) ;
#6235 = ADVANCED_FACE ( 'NONE', ( #12499 ), #15141, .F. ) ;
#6236 = ORIENTED_EDGE ( 'NONE', *, *, #4056, .F. ) ;
#6237 = CARTESIAN_POINT ( 'NONE',  ( 33.36777657078724957, 191.6397216241468300, -28.71272404723382721 ) ) ;
#6238 = CARTESIAN_POINT ( 'NONE',  ( 30.00000000000001066, 146.6227766016838245, 0.000000000000000000 ) ) ;
#6239 = CONICAL_SURFACE ( 'NONE', #4840, 33.26794919243112503, 0.5235987755983005920 ) ;
#6240 = ORIENTED_EDGE ( 'NONE', *, *, #14369, .F. ) ;
#6241 = ORIENTED_EDGE ( 'NONE', *, *, #10061, .F. ) ;
#6242 = AXIS2_PLACEMENT_3D ( 'NONE', #12694, #8710, #4558 ) ;
#6243 = CARTESIAN_POINT ( 'NONE',  ( -74.91436539010484807, 152.1411297330830052, -26.63673872167001377 ) ) ;
#6244 = ORIENTED_EDGE ( 'NONE', *, *, #9944, .F. ) ;
#6245 = SURFACE_STYLE_FILL_AREA ( #6413 ) ;
#6246 = CARTESIAN_POINT ( 'NONE',  ( -16.17053951239850207, 32.72994544565565889, 6.425226171708652956 ) ) ;
#6247 =( NAMED_UNIT ( * ) SI_UNIT ( $, .STERADIAN. ) SOLID_ANGLE_UNIT ( ) );
#6248 = DIRECTION ( 'NONE',  ( 0.000000000000000000, 0.000000000000000000, -1.000000000000000000 ) ) ;
#6249 = AXIS2_PLACEMENT_3D ( 'NONE', #12606, #1807, #9680 ) ;
#6250 = CARTESIAN_POINT ( 'NONE',  ( 22.93524650466160253, 29.84210526315789025, 5.000000000000003553 ) ) ;
#6251 = CARTESIAN_POINT ( 'NONE',  ( 15.56337975240373162, 125.2134999403455851, 5.000000000000083489 ) ) ;
#6252 = ORIENTED_EDGE ( 'NONE', *, *, #719, .T. ) ;
#6253 = CARTESIAN_POINT ( 'NONE',  ( 18.93231600135347392, 142.3609111598534298, 15.26062816855829851 ) ) ;
#6254 = CARTESIAN_POINT ( 'NONE',  ( 0.000000000000000000, -20.00000000000000000, 0.000000000000000000 ) ) ;
#6255 = ADVANCED_FACE ( 'NONE', ( #8422 ), #7364, .F. ) ;
#6256 = CARTESIAN_POINT ( 'NONE',  ( 34.93420767853316988, 30.00000000000000000, 15.00000000000000000 ) ) ;
#6257 = DIRECTION ( 'NONE',  ( -1.000000000000000000, 0.000000000000000000, 2.312964634635742464E-16 ) ) ;
#6258 = EDGE_CURVE ( 'NONE', #8416, #12853, #17430, .T. ) ;
#6259 = CARTESIAN_POINT ( 'NONE',  ( 14.93242934743711992, 18.00000000000000355, 25.00000000000000000 ) ) ;
#6260 = VECTOR ( 'NONE', #4356, 1000.000000000000000 ) ;
#6261 = CARTESIAN_POINT ( 'NONE',  ( -80.00000000000001421, 196.6227766016838245, 0.000000000000000000 ) ) ;
#6262 = EDGE_LOOP ( 'NONE', ( #16312, #5897 ) ) ;
#6263 = FILL_AREA_STYLE ('',( #3776 ) ) ;
#6264 = CARTESIAN_POINT ( 'NONE',  ( -82.50000000000001421, 196.6227766016838245, 1.387778780781445676E-14 ) ) ;
#6265 = EDGE_LOOP ( 'NONE', ( #8080, #14588, #3915, #3303, #5725, #8757 ) ) ;
#6266 = CARTESIAN_POINT ( 'NONE',  ( -85.97513963119602920, 195.9845216101233802, -25.13379275193914353 ) ) ;
#6267 = CARTESIAN_POINT ( 'NONE',  ( -27.98221281347037603, 18.00000000000000000, 0.000000000000000000 ) ) ;
#6268 = ADVANCED_FACE ( 'NONE', ( #3113 ), #8777, .F. ) ;
#6269 = CARTESIAN_POINT ( 'NONE',  ( 15.41470791700940879, 125.6764093509959963, -6.286214449974339757 ) ) ;
#6270 = ORIENTED_EDGE ( 'NONE', *, *, #4223, .F. ) ;
#6271 = FACE_OUTER_BOUND ( 'NONE', #8841, .T. ) ;
#6272 = DIRECTION ( 'NONE',  ( 1.000000000000000000, -0.000000000000000000, -0.000000000000000000 ) ) ;
#6273 = DIRECTION ( 'NONE',  ( 0.000000000000000000, 1.000000000000000000, 0.000000000000000000 ) ) ;
#6274 = CARTESIAN_POINT ( 'NONE',  ( 29.09190978889357737, 202.5550951275239413, -16.37659873159347512 ) ) ;
#6275 = VERTEX_POINT ( 'NONE', #8515 ) ;
#6276 = ORIENTED_EDGE ( 'NONE', *, *, #1796, .F. ) ;
#6277 = CARTESIAN_POINT ( 'NONE',  ( 16.23418548573199516, 29.98246013044581915, -14.93677958672484785 ) ) ;
#6278 = CARTESIAN_POINT ( 'NONE',  ( 12.89436750745977278, 141.9634372303913779, -18.58317047499899743 ) ) ;
#6279 = VERTEX_POINT ( 'NONE', #12582 ) ;
#6280 = CARTESIAN_POINT ( 'NONE',  ( 39.99999999999998579, 8.648601236627303230E-15, 33.00000000000001421 ) ) ;
#6281 = DIRECTION ( 'NONE',  ( 1.000000000000000000, 0.000000000000000000, 0.000000000000000000 ) ) ;
#6282 = VERTEX_POINT ( 'NONE', #8690 ) ;
#6283 = PLANE ( 'NONE',  #13852 ) ;
#6284 = ADVANCED_FACE ( 'NONE', ( #1875 ), #549, .T. ) ;
#6285 = DIRECTION ( 'NONE',  ( 0.000000000000000000, 0.000000000000000000, 1.000000000000000000 ) ) ;
#6286 = DIRECTION ( 'NONE',  ( -1.000000000000000000, -0.000000000000000000, -0.000000000000000000 ) ) ;
#6287 = CARTESIAN_POINT ( 'NONE',  ( -9.245637070518823109, 17.99999999999769074, 12.12237611798427572 ) ) ;
#6288 = DIRECTION ( 'NONE',  ( -0.000000000000000000, -0.000000000000000000, -1.000000000000000000 ) ) ;
#6289 = CARTESIAN_POINT ( 'NONE',  ( 28.70390606474517625, 140.7594520581394022, -16.50672721711050528 ) ) ;
#6290 = ORIENTED_EDGE ( 'NONE', *, *, #12388, .T. ) ;
#6291 = CARTESIAN_POINT ( 'NONE',  ( -80.00000000000002842, 146.6227766016838245, 10.00000000000000178 ) ) ;
#6292 = ORIENTED_EDGE ( 'NONE', *, *, #14162, .T. ) ;
#6293 = EDGE_CURVE ( 'NONE', #16965, #17478, #15164, .T. ) ;
#6294 = DIRECTION ( 'NONE',  ( 1.000000000000000000, 0.000000000000000000, 0.000000000000000000 ) ) ;
#6295 = EDGE_CURVE ( 'NONE', #4586, #17341, #14879, .T. ) ;
#6296 = FACE_BOUND ( 'NONE', #2400, .T. ) ;
#6297 = ORIENTED_EDGE ( 'NONE', *, *, #8085, .F. ) ;
#6298 = CARTESIAN_POINT ( 'NONE',  ( 32.29638371061065527, 20.00000000000000355, 15.01265034258821096 ) ) ;
#6299 = CARTESIAN_POINT ( 'NONE',  ( 10.22516481506617581, 140.0471213951830407, 11.75777818883246617 ) ) ;
#6300 = CARTESIAN_POINT ( 'NONE',  ( 27.13959012325755538, 19.99999999999999645, 20.89788123228700556 ) ) ;
#6301 = ORIENTED_EDGE ( 'NONE', *, *, #7385, .T. ) ;
#6302 = CARTESIAN_POINT ( 'NONE',  ( 15.00000000000000000, 143.0344144757318929, 16.50549856913627877 ) ) ;
#6303 = FACE_OUTER_BOUND ( 'NONE', #7453, .T. ) ;
#6304 = FACE_BOUND ( 'NONE', #5027, .T. ) ;
#6305 = CARTESIAN_POINT ( 'NONE',  ( -17.59086657693884703, 18.00000000000000000, -22.42595686383721443 ) ) ;
#6306 = PRODUCT_RELATED_PRODUCT_CATEGORY ( 'part', '', ( #15205 ) ) ;
#6307 = ORIENTED_EDGE ( 'NONE', *, *, #8799, .T. ) ;
#6308 = DIRECTION ( 'NONE',  ( 0.000000000000000000, 1.000000000000000000, 0.000000000000000000 ) ) ;
#6309 = ORIENTED_EDGE ( 'NONE', *, *, #9874, .F. ) ;
#6310 = CARTESIAN_POINT ( 'NONE',  ( 35.39974920818285398, 194.0006876528842668, -26.91236748077486141 ) ) ;
#6311 = DIRECTION ( 'NONE',  ( 0.9961946980917461003, 0.08715574274765185148, 0.000000000000000000 ) ) ;
#6312 =( BOUNDED_CURVE ( )  B_SPLINE_CURVE ( 3, ( #14352, #14444, #17273, #17355 ),
 .UNSPECIFIED., .F., .F. ) 
 B_SPLINE_CURVE_WITH_KNOTS ( ( 4, 4 ),
 ( 3.141592653589792672, 4.712388980384690562 ),
 .UNSPECIFIED. ) 
 CURVE ( )  GEOMETRIC_REPRESENTATION_ITEM ( )  RATIONAL_B_SPLINE_CURVE ( ( 1.000000000000000000, 0.8047378541243646044, 0.8047378541243646044, 1.000000000000000000 ) ) 
 REPRESENTATION_ITEM ( '' )  );
#6313 = VERTEX_POINT ( 'NONE', #723 ) ;
#6314 = ORIENTED_EDGE ( 'NONE', *, *, #16708, .T. ) ;
#6315 = EDGE_LOOP ( 'NONE', ( #5902, #3159, #9035, #3480, #1692, #16838 ) ) ;
#6316 = CARTESIAN_POINT ( 'NONE',  ( -76.18268817859248543, 153.1022248993911887, -27.31438289289432220 ) ) ;
#6317 = B_SPLINE_CURVE_WITH_KNOTS ( 'NONE', 3,
 ( #13342, #14666, #1206, #2630, #14488, #16181, #10403, #6609, #3966, #5279 ),
 .UNSPECIFIED., .F., .F.,
 ( 4, 2, 2, 2, 4 ),
 ( 0.03775390620236027117, 0.04033669301524707429, 0.04291947982813387741, 0.04550226664102068053, 0.04808505345390748364 ),
 .UNSPECIFIED. ) ;
#6318 = ORIENTED_EDGE ( 'NONE', *, *, #3483, .T. ) ;
#6319 = EDGE_CURVE ( 'NONE', #12075, #7078, #16491, .T. ) ;
#6320 = DIRECTION ( 'NONE',  ( 0.000000000000000000, 0.000000000000000000, -1.000000000000000000 ) ) ;
#6321 = CARTESIAN_POINT ( 'NONE',  ( -3.000000000000002665, 144.1839557653416080, 18.33333333333336057 ) ) ;
#6322 = CARTESIAN_POINT ( 'NONE',  ( 34.30925017698373836, 150.8166157800934570, -28.14689102807276555 ) ) ;
#6323 = CARTESIAN_POINT ( 'NONE',  ( 34.80444759354871564, 18.00000000000000000, 7.621511755358874929 ) ) ;
#6324 = CARTESIAN_POINT ( 'NONE',  ( -208.0000000000000853, 170.0678595944000620, -2.693195258168412654 ) ) ;
#6325 = VECTOR ( 'NONE', #16950, 1000.000000000000000 ) ;
#6326 = ORIENTED_EDGE ( 'NONE', *, *, #6959, .F. ) ;
#6327 = CYLINDRICAL_SURFACE ( 'NONE', #15207, 5.000000000000000888 ) ;
#6328 = CYLINDRICAL_SURFACE ( 'NONE', #418, 33.00000000000000000 ) ;
#6330 = CYLINDRICAL_SURFACE ( 'NONE', #5100, 12.00000000000000000 ) ;
#6329 = CIRCLE ( 'NONE', #5498, 10.00000000000000178 ) ;
#6331 = CARTESIAN_POINT ( 'NONE',  ( -26.90043998676167192, 19.99999999999999645, -11.53672424425260878 ) ) ;
#6332 = ORIENTED_EDGE ( 'NONE', *, *, #455, .T. ) ;
#6333 = DIRECTION ( 'NONE',  ( 0.9961946980917461003, 0.08715574274765185148, 0.000000000000000000 ) ) ;
#6334 = CARTESIAN_POINT ( 'NONE',  ( 31.70991205391183954, 201.3251192758334298, 14.38044245167808022 ) ) ;
#6335 = EDGE_LOOP ( 'NONE', ( #13668, #4034, #2899, #7666 ) ) ;
#6336 = DIRECTION ( 'NONE',  ( -0.000000000000000000, -0.000000000000000000, -1.000000000000000000 ) ) ;
#6337 = DIRECTION ( 'NONE',  ( -0.000000000000000000, 0.000000000000000000, -1.000000000000000000 ) ) ;
#6338 = CIRCLE ( 'NONE', #7479, 2.055000000000000160 ) ;
#6339 = ORIENTED_EDGE ( 'NONE', *, *, #17017, .T. ) ;
#6340 = EDGE_CURVE ( 'NONE', #16539, #152, #13104, .T. ) ;
#6341 = EDGE_CURVE ( 'NONE', #9911, #16300, #17268, .T. ) ;
#6342 = CARTESIAN_POINT ( 'NONE',  ( -151.0000000000000284, 171.6227766016838245, 0.000000000000000000 ) ) ;
#6343 = ADVANCED_FACE ( 'NONE', ( #970 ), #11602, .F. ) ;
#6344 = EDGE_CURVE ( 'NONE', #16020, #15739, #3640, .T. ) ;
#6345 = FACE_OUTER_BOUND ( 'NONE', #2058, .T. ) ;
#6346 = DIRECTION ( 'NONE',  ( 1.000000000000000000, 0.000000000000000000, 0.000000000000000000 ) ) ;
#6347 = CARTESIAN_POINT ( 'NONE',  ( -168.0000000000000284, 168.3180863238818006, -5.723891464432168341 ) ) ;
#6348 = ORIENTED_EDGE ( 'NONE', *, *, #12515, .F. ) ;
#6349 = CARTESIAN_POINT ( 'NONE',  ( 22.93524650466158832, 29.84210526315789380, 0.000000000000000000 ) ) ;
#6350 = DIRECTION ( 'NONE',  ( 0.000000000000000000, -1.000000000000000000, 0.000000000000000000 ) ) ;
#6351 = DIRECTION ( 'NONE',  ( 0.000000000000000000, 0.000000000000000000, 1.000000000000000000 ) ) ;
#6352 = CARTESIAN_POINT ( 'NONE',  ( 33.63492343075080271, 201.4000939832746155, -18.39459910103779450 ) ) ;
#6353 = AXIS2_PLACEMENT_3D ( 'NONE', #14008, #12583, #4449 ) ;
#6354 = ORIENTED_EDGE ( 'NONE', *, *, #4333, .F. ) ;
#6355 = AXIS2_PLACEMENT_3D ( 'NONE', #16114, #5302, #5127 ) ;
#6356 = ORIENTED_EDGE ( 'NONE', *, *, #3098, .F. ) ;
#6357 = FACE_OUTER_BOUND ( 'NONE', #17082, .T. ) ;
#6358 = ORIENTED_EDGE ( 'NONE', *, *, #14502, .T. ) ;
#6359 = DIRECTION ( 'NONE',  ( -1.000000000000000000, 0.000000000000000000, 0.000000000000000000 ) ) ;
#6360 = ORIENTED_EDGE ( 'NONE', *, *, #4592, .F. ) ;
#6361 = DIRECTION ( 'NONE',  ( 0.000000000000000000, -0.000000000000000000, 1.000000000000000000 ) ) ;
#6362 = CARTESIAN_POINT ( 'NONE',  ( 15.07980489400154056, 126.2730657262978724, -7.274180996386617970 ) ) ;
#6363 = EDGE_LOOP ( 'NONE', ( #16224, #6631, #11896, #16748 ) ) ;
#6364 = CARTESIAN_POINT ( 'NONE',  ( -168.3486229709906183, 166.3256969276982034, 9.174811127083433604 ) ) ;
#6365 = CIRCLE ( 'NONE', #12036, 7.500000000000000000 ) ;
#6366 = DIRECTION ( 'NONE',  ( -1.000000000000000000, 0.000000000000000000, 0.000000000000000000 ) ) ;
#6367 = VECTOR ( 'NONE', #5188, 1000.000000000000000 ) ;
#6368 = CARTESIAN_POINT ( 'NONE',  ( 34.07008595419463148, 193.7005638513908536, 24.52922227238014941 ) ) ;
#6369 = VECTOR ( 'NONE', #4844, 1000.000000000000000 ) ;
#6370 = CARTESIAN_POINT ( 'NONE',  ( 196.0000000000000000, 151.6227766016839098, 5.571800142134973655 ) ) ;
#6371 = DIRECTION ( 'NONE',  ( 0.000000000000000000, 0.000000000000000000, -1.000000000000000000 ) ) ;
#6372 = VECTOR ( 'NONE', #13421, 1000.000000000000000 ) ;
#6373 = CARTESIAN_POINT ( 'NONE',  ( -19.80886414215282798, 18.00000000000000000, 20.97268729564153489 ) ) ;
#6374 = FACE_OUTER_BOUND ( 'NONE', #11913, .T. ) ;
#6375 = DIRECTION ( 'NONE',  ( 0.000000000000000000, 1.000000000000000000, 0.000000000000000000 ) ) ;
#6376 = ORIENTED_EDGE ( 'NONE', *, *, #16047, .T. ) ;
#6377 = CARTESIAN_POINT ( 'NONE',  ( 39.99999999999998579, 20.00000000000000000, 30.00000000000001066 ) ) ;
#6378 = ORIENTED_EDGE ( 'NONE', *, *, #9107, .T. ) ;
#6379 = CARTESIAN_POINT ( 'NONE',  ( 1.559999999999998943, -0.8660254037844428154, 1.500000000000001332 ) ) ;
#6380 = CLOSED_SHELL ( 'NONE', ( #5813, #13369, #6205, #16486, #17351, #15245, #13690, #15493, #10124, #8032, #13534, #5173, #2567, #2200, #5316, #2396 ) ) ;
#6381 = CARTESIAN_POINT ( 'NONE',  ( -22.79696676584440596, 18.00000000000000711, -18.34105320469107170 ) ) ;
#6382 = EDGE_CURVE ( 'NONE', #16806, #588, #5142, .T. ) ;
#6383 = AXIS2_PLACEMENT_3D ( 'NONE', #16611, #9870, #8195 ) ;
#6384 = ORIENTED_EDGE ( 'NONE', *, *, #13556, .F. ) ;
#6385 = EDGE_CURVE ( 'NONE', #2044, #12997, #3294, .T. ) ;
#6386 = CARTESIAN_POINT ( 'NONE',  ( -19.80886414215398261, 19.99999999999999645, 20.97268729564270728 ) ) ;
#6387 = CARTESIAN_POINT ( 'NONE',  ( 21.38051303318334462, 141.6185065902053282, 13.74313897096208414 ) ) ;
#6388 = CARTESIAN_POINT ( 'NONE',  ( -48.00000000000000000, 204.6227766016838245, 0.000000000000000000 ) ) ;
#6389 = ORIENTED_EDGE ( 'NONE', *, *, #12004, .F. ) ;
#6390 = DIRECTION ( 'NONE',  ( 1.000000000000000000, 0.000000000000000000, -0.000000000000000000 ) ) ;
#6391 = ADVANCED_FACE ( 'NONE', ( #2481 ), #7526, .F. ) ;
#6392 = CIRCLE ( 'NONE', #7530, 40.99999999999997868 ) ;
#6393 = AXIS2_PLACEMENT_3D ( 'NONE', #7613, #10350, #14609 ) ;
#6394 = PLANE ( 'NONE',  #1672 ) ;
#6395 = DIRECTION ( 'NONE',  ( 0.000000000000000000, 0.9938079899999064937, 0.1111111111111109523 ) ) ;
#6396 = AXIS2_PLACEMENT_3D ( 'NONE', #4515, #7248, #858 ) ;
#6397 = CARTESIAN_POINT ( 'NONE',  ( -12.54944958582184888, 31.64997543288135873, -11.54276402733058937 ) ) ;
#6398 = AXIS2_PLACEMENT_3D ( 'NONE', #4070, #4155, #16547 ) ;
#6399 = EDGE_LOOP ( 'NONE', ( #10043, #11550, #8221, #1513 ) ) ;
#6400 = CARTESIAN_POINT ( 'NONE',  ( -725.0000000000000000, 19.99999999999995737, -15.00000000000000000 ) ) ;
#6401 = EDGE_LOOP ( 'NONE', ( #12213, #5941, #15271, #5160, #879 ) ) ;
#6402 = CARTESIAN_POINT ( 'NONE',  ( -85.00000000000002842, 146.6227766016838245, 0.000000000000000000 ) ) ;
#6403 = CARTESIAN_POINT ( 'NONE',  ( -87.50000000000004263, 196.6227766016838245, -21.54065922853802562 ) ) ;
#6404 = EDGE_LOOP ( 'NONE', ( #11432, #16201, #1369, #695 ) ) ;
#6405 = ORIENTED_EDGE ( 'NONE', *, *, #10983, .F. ) ;
#6406 = ORIENTED_EDGE ( 'NONE', *, *, #9562, .T. ) ;
#6407 = VECTOR ( 'NONE', #10257, 1000.000000000000000 ) ;
#6408 = AXIS2_PLACEMENT_3D ( 'NONE', #11135, #15480, #13987 ) ;
#6409 = AXIS2_PLACEMENT_3D ( 'NONE', #2465, #1045, #15832 ) ;
#6410 = CARTESIAN_POINT ( 'NONE',  ( -75.73052444394195959, 152.8115259536291148, -27.11642929875282348 ) ) ;
#6411 = CIRCLE ( 'NONE', #475, 30.00000000000000000 ) ;
#6412 = ORIENTED_EDGE ( 'NONE', *, *, #12482, .T. ) ;
#6413 = FILL_AREA_STYLE ('',( #10566 ) ) ;
#6414 = CARTESIAN_POINT ( 'NONE',  ( -11.59473107857741425, 31.35552539902487723, 12.08231249604354574 ) ) ;
#6415 = EDGE_CURVE ( 'NONE', #9250, #6665, #2386, .T. ) ;
#6416 = CARTESIAN_POINT ( 'NONE',  ( -73.00000000000001421, 171.6227766016838245, -19.49999999999998934 ) ) ;
#6417 = EDGE_CURVE ( 'NONE', #938, #7945, #17176, .T. ) ;
#6418 = CARTESIAN_POINT ( 'NONE',  ( 24.10468692392765533, 147.7508872708765750, -25.59654897292658049 ) ) ;
#6419 = CARTESIAN_POINT ( 'NONE',  ( 22.12396056536369215, 29.85772992373802026, 8.548742771607255264 ) ) ;
#6420 = DIRECTION ( 'NONE',  ( -1.000000000000000000, 0.000000000000000000, -8.673617379884036705E-17 ) ) ;
#6421 = ORIENTED_EDGE ( 'NONE', *, *, #9625, .T. ) ;
#6422 = DIRECTION ( 'NONE',  ( -1.000000000000000000, -0.000000000000000000, -0.000000000000000000 ) ) ;
#6423 = LINE ( 'NONE', #2268, #8895 ) ;
#6424 = CIRCLE ( 'NONE', #5306, 4.000000000000001776 ) ;
#6425 = LINE ( 'NONE', #864, #14159 ) ;
#6426 = ORIENTED_EDGE ( 'NONE', *, *, #17427, .T. ) ;
#6427 = DIRECTION ( 'NONE',  ( 1.000000000000000000, 0.000000000000000000, 0.000000000000000000 ) ) ;
#6428 = CARTESIAN_POINT ( 'NONE',  ( -27.99999999999998224, 4.000000000000000000, -30.00000000000000711 ) ) ;
#6429 = ORIENTED_EDGE ( 'NONE', *, *, #16758, .F. ) ;
#6430 = DIRECTION ( 'NONE',  ( -0.000000000000000000, -0.000000000000000000, -1.000000000000000000 ) ) ;
#6431 = CIRCLE ( 'NONE', #14340, 6.000000000000005329 ) ;
#6432 = EDGE_CURVE ( 'NONE', #6602, #13323, #14601, .T. ) ;
#6433 = CARTESIAN_POINT ( 'NONE',  ( 34.01316144709517886, 199.6193856840139063, 17.47499078086477553 ) ) ;
#6434 = ORIENTED_EDGE ( 'NONE', *, *, #5703, .T. ) ;
#6435 = FILL_AREA_STYLE_COLOUR ( '', #2463 ) ;
#6436 = DIRECTION ( 'NONE',  ( 1.000000000000000000, 0.000000000000000000, 0.000000000000000000 ) ) ;
#6437 = ORIENTED_EDGE ( 'NONE', *, *, #14467, .F. ) ;
#6438 = CARTESIAN_POINT ( 'NONE',  ( -83.43212945347822540, 142.9736659102426870, 16.38272693053711393 ) ) ;
#6439 = CIRCLE ( 'NONE', #3333, 2.499999999999998668 ) ;
#6440 = DIRECTION ( 'NONE',  ( 0.000000000000000000, 0.000000000000000000, -1.000000000000000000 ) ) ;
#6441 = CARTESIAN_POINT ( 'NONE',  ( -86.00000000000001421, 146.2509476181505477, -24.11540106065089262 ) ) ;
#6442 = DIRECTION ( 'NONE',  ( -1.000000000000000000, -0.000000000000000000, -0.000000000000000000 ) ) ;
#6443 = VERTEX_POINT ( 'NONE', #15589 ) ;
#6444 = CARTESIAN_POINT ( 'NONE',  ( -5.000000000000000888, 171.6227766016838245, 0.000000000000000000 ) ) ;
#6445 = CARTESIAN_POINT ( 'NONE',  ( -208.1430079281944074, 172.4097984991905435, -5.932774073184737595 ) ) ;
#6446 = CARTESIAN_POINT ( 'NONE',  ( 0.000000000000000000, -0.8660254037844428154, 1.500000000000001332 ) ) ;
#6447 = DIRECTION ( 'NONE',  ( 0.000000000000000000, 0.000000000000000000, 1.000000000000000000 ) ) ;
#6448 = EDGE_CURVE ( 'NONE', #4054, #12800, #1603, .T. ) ;
#6449 = ADVANCED_FACE ( 'NONE', ( #9030 ), #15758, .F. ) ;
#6450 = VECTOR ( 'NONE', #10575, 1000.000000000000114 ) ;
#6451 = EDGE_CURVE ( 'NONE', #13930, #10657, #13763, .T. ) ;
#6452 = ORIENTED_EDGE ( 'NONE', *, *, #4182, .T. ) ;
#6453 = AXIS2_PLACEMENT_3D ( 'NONE', #2306, #14118, #6366 ) ;
#6454 = ORIENTED_EDGE ( 'NONE', *, *, #17382, .F. ) ;
#6455 = FACE_OUTER_BOUND ( 'NONE', #1595, .T. ) ;
#6456 = ORIENTED_EDGE ( 'NONE', *, *, #4843, .F. ) ;
#6457 = CARTESIAN_POINT ( 'NONE',  ( 196.0000000000000000, 159.6227766016838814, 3.071800142134975431 ) ) ;
#6458 = CARTESIAN_POINT ( 'NONE',  ( 11.61604111307750209, 130.6582085322020532, -11.34316963496758390 ) ) ;
#6459 = EDGE_LOOP ( 'NONE', ( #8751, #3686, #888, #5772 ) ) ;
#6460 = CARTESIAN_POINT ( 'NONE',  ( 30.49999999999998224, 9.999999999999998224, -16.00000000000000000 ) ) ;
#6461 = CARTESIAN_POINT ( 'NONE',  ( -3.000000000000000888, 171.6227766016838245, 0.000000000000000000 ) ) ;
#6462 = DIRECTION ( 'NONE',  ( 0.000000000000000000, 1.000000000000000000, 0.000000000000000000 ) ) ;
#6463 = CIRCLE ( 'NONE', #7315, 10.00000000000000178 ) ;
#6464 = CARTESIAN_POINT ( 'NONE',  ( 35.00000000000000000, 196.6227766016838245, 21.54065922853802206 ) ) ;
#6465 = VECTOR ( 'NONE', #7501, 1000.000000000000000 ) ;
#6466 = CARTESIAN_POINT ( 'NONE',  ( 0.000000000000000000, 0.000000000000000000, -33.00000000000000711 ) ) ;
#6467 = FACE_OUTER_BOUND ( 'NONE', #9282, .T. ) ;
#6468 = CARTESIAN_POINT ( 'NONE',  ( -5.000000000000004441, 142.8100939375178200, -16.63501009223129756 ) ) ;
#6469 = LINE ( 'NONE', #12043, #821 ) ;
#6470 = DIRECTION ( 'NONE',  ( 0.000000000000000000, 0.000000000000000000, 1.000000000000000000 ) ) ;
#6471 = CARTESIAN_POINT ( 'NONE',  ( 34.99061305271412436, 143.2738031352136545, -20.53261660472919203 ) ) ;
#6472 = VERTEX_POINT ( 'NONE', #17084 ) ;
#6473 = DIRECTION ( 'NONE',  ( 8.673617379884037937E-17, 0.000000000000000000, 1.000000000000000000 ) ) ;
#6474 = ADVANCED_FACE ( 'NONE', ( #14258 ), #10264, .F. ) ;
#6476 = VERTEX_POINT ( 'NONE', #2125 ) ;
#6475 = VECTOR ( 'NONE', #9778, 1000.000000000000000 ) ;
#6477 = DIRECTION ( 'NONE',  ( -1.000000000000000000, 0.000000000000000000, 0.000000000000000000 ) ) ;
#6478 = VECTOR ( 'NONE', #1337, 1000.000000000000000 ) ;
#6479 = LINE ( 'NONE', #10726, #3581 ) ;
#6480 = AXIS2_PLACEMENT_3D ( 'NONE', #9492, #15066, #13585 ) ;
#6481 = ORIENTED_EDGE ( 'NONE', *, *, #17060, .F. ) ;
#6482 = DIRECTION ( 'NONE',  ( 0.000000000000000000, 1.000000000000000000, 0.000000000000000000 ) ) ;
#6483 = CARTESIAN_POINT ( 'NONE',  ( 13.00433657606611604, 139.2454419355441928, 9.442801289196161463 ) ) ;
#6484 = ORIENTED_EDGE ( 'NONE', *, *, #1597, .T. ) ;
#6485 = CARTESIAN_POINT ( 'NONE',  ( 14.93242934743711814, 20.00000000000000000, 24.99999999999999645 ) ) ;
#6486 = ORIENTED_EDGE ( 'NONE', *, *, #7972, .F. ) ;
#6487 = CARTESIAN_POINT ( 'NONE',  ( 48.00000000000000711, 171.6227766016838245, 0.000000000000000000 ) ) ;
#6488 = CARTESIAN_POINT ( 'NONE',  ( 24.54894360611539028, 191.4650750923992177, -26.36917907415269013 ) ) ;
#6489 = VECTOR ( 'NONE', #11648, 1000.000000000000000 ) ;
#6490 = CARTESIAN_POINT ( 'NONE',  ( 27.44407568426044008, 126.9014170516880284, -4.999999999999997335 ) ) ;
#6491 = CARTESIAN_POINT ( 'NONE',  ( -10.13698291596435119, 17.99999999999999645, -11.46558158188963539 ) ) ;
#6492 = EDGE_CURVE ( 'NONE', #11986, #16166, #812, .T. ) ;
#6493 = CIRCLE ( 'NONE', #16405, 5.000000000000000888 ) ;
#6494 = ORIENTED_EDGE ( 'NONE', *, *, #15639, .F. ) ;
#6495 = DIRECTION ( 'NONE',  ( -0.9940220915700700433, -0.05458956280888926926, -0.09455189634797064868 ) ) ;
#6496 = EDGE_LOOP ( 'NONE', ( #4655, #3007 ) ) ;
#6497 = CARTESIAN_POINT ( 'NONE',  ( 24.27133314458328428, 194.8302331505971665, -26.20043099198421288 ) ) ;
#6498 = CARTESIAN_POINT ( 'NONE',  ( -85.27494917608791525, 201.9542783778900059, -13.00000000000000000 ) ) ;
#6499 = ORIENTED_EDGE ( 'NONE', *, *, #6295, .F. ) ;
#6500 = ORIENTED_EDGE ( 'NONE', *, *, #3936, .F. ) ;
#6501 = EDGE_LOOP ( 'NONE', ( #9364, #13451, #16033, #2588 ) ) ;
#6502 = AXIS2_PLACEMENT_3D ( 'NONE', #780, #14234, #16891 ) ;
#6503 = VECTOR ( 'NONE', #6740, 1000.000000000000000 ) ;
#6504 = FACE_OUTER_BOUND ( 'NONE', #13919, .T. ) ;
#6505 = UNCERTAINTY_MEASURE_WITH_UNIT (LENGTH_MEASURE( 1.000000000000000082E-05 ), #6976, 'distance_accuracy_value', 'NONE');
#6506 = VECTOR ( 'NONE', #16810, 1000.000000000000000 ) ;
#6507 = EDGE_LOOP ( 'NONE', ( #10396, #3232, #6027, #8315 ) ) ;
#6508 = DIRECTION ( 'NONE',  ( 0.000000000000000000, 0.000000000000000000, 1.000000000000000000 ) ) ;
#6509 = DIRECTION ( 'NONE',  ( 1.000000000000000000, 0.000000000000000000, 0.000000000000000000 ) ) ;
#6510 = CARTESIAN_POINT ( 'NONE',  ( -8.058782516633090864, 30.15486961025272450, 15.00000000000000178 ) ) ;
#6511 = CARTESIAN_POINT ( 'NONE',  ( 24.13838555012902276, 147.9152928535323213, -25.74888847741386044 ) ) ;
#6512 = CARTESIAN_POINT ( 'NONE',  ( 29.53214135918722505, 18.00000000000000000, 18.68621337607990185 ) ) ;
#6513 = PLANE ( 'NONE',  #16560 ) ;
#6514 = EDGE_CURVE ( 'NONE', #3772, #13139, #17009, .T. ) ;
#6515 = ORIENTED_EDGE ( 'NONE', *, *, #11929, .F. ) ;
#6516 = CARTESIAN_POINT ( 'NONE',  ( -100.0000000000000000, 100.0000000000000142, -6.000000000000000000 ) ) ;
#6517 = VECTOR ( 'NONE', #11818, 1000.000000000000000 ) ;
#6518 = PLANE ( 'NONE',  #13707 ) ;
#6519 = CARTESIAN_POINT ( 'NONE',  ( 16.97539380423070909, 126.5649914159620266, 7.928130581088665529 ) ) ;
#6520 = CYLINDRICAL_SURFACE ( 'NONE', #1578, 27.69059892324149530 ) ;
#6521 = AXIS2_PLACEMENT_3D ( 'NONE', #11638, #17043, #6320 ) ;
#6522 = CARTESIAN_POINT ( 'NONE',  ( -18.18164784767110120, 32.29378831700660157, -6.323624269675778287 ) ) ;
#6523 = VERTEX_POINT ( 'NONE', #10446 ) ;
#6524 = CARTESIAN_POINT ( 'NONE',  ( 30.00000000000001066, 146.6227766016838245, 0.000000000000000000 ) ) ;
#6525 = B_SPLINE_CURVE_WITH_KNOTS ( 'NONE', 3,
 ( #17309, #6510, #9151, #2342, #17125, #14557, #16075, #7732, #2430, #11901, #5177, #14394, #14746, #3955, #10568, #3589, #8004, #3858, #6598, #7655, #9246, #13411, #14653, #10300, #13065, #2531 ),
 .UNSPECIFIED., .F., .F.,
 ( 4, 2, 2, 2, 2, 2, 2, 2, 2, 2, 2, 2, 4 ),
 ( 0.000000000000000000, 0.002066677509289960735, 0.003100016263934941754, 0.004133355018579923205, 0.006200032527869886109, 0.007233371282514866260, 0.008266710037159848146, 0.01033338754644981018, 0.01136672630109478513, 0.01240006505573976354, 0.01446674256502970997, 0.01550008131967467971, 0.01653342007431965119 ),
 .UNSPECIFIED. ) ;
#6526 = EDGE_CURVE ( 'NONE', #13081, #4701, #12633, .T. ) ;
#6527 = EDGE_CURVE ( 'NONE', #12225, #8437, #13199, .T. ) ;
#6528 = EDGE_CURVE ( 'NONE', #16562, #4758, #16211, .T. ) ;
#6529 = CARTESIAN_POINT ( 'NONE',  ( 25.00000000000000000, 196.6227766016838245, 21.54065922853802562 ) ) ;
#6530 = VERTEX_POINT ( 'NONE', #5319 ) ;
#6531 = CARTESIAN_POINT ( 'NONE',  ( -32.14917720409751922, 100.1152149123505239, -5.472305571546616676 ) ) ;
#6532 = DIRECTION ( 'NONE',  ( 0.000000000000000000, 0.000000000000000000, 1.000000000000000000 ) ) ;
#6533 = AXIS2_PLACEMENT_3D ( 'NONE', #4736, #8967, #7464 ) ;
#6534 = ORIENTED_EDGE ( 'NONE', *, *, #7414, .F. ) ;
#6535 = FILL_AREA_STYLE ('',( #7849 ) ) ;
#6536 = FACE_OUTER_BOUND ( 'NONE', #8429, .T. ) ;
#6537 = CYLINDRICAL_SURFACE ( 'NONE', #7777, 4.999999999999997335 ) ;
#6538 = CARTESIAN_POINT ( 'NONE',  ( -79.72426293143250575, 140.6276388071887880, -16.25736180127251629 ) ) ;
#6539 = CARTESIAN_POINT ( 'NONE',  ( -7.379000772444994638, 20.00000000000000000, 25.00000000000000000 ) ) ;
#6540 = EDGE_LOOP ( 'NONE', ( #819, #14646 ) ) ;
#6541 = CARTESIAN_POINT ( 'NONE',  ( 37.99999999999999289, 2.000000000000000000, 0.000000000000000000 ) ) ;
#6542 = FACE_OUTER_BOUND ( 'NONE', #8787, .T. ) ;
#6543 = FACE_OUTER_BOUND ( 'NONE', #9128, .T. ) ;
#6544 = AXIS2_PLACEMENT_3D ( 'NONE', #4642, #4299, #577 ) ;
#6545 = ORIENTED_EDGE ( 'NONE', *, *, #11421, .F. ) ;
#6546 = ORIENTED_EDGE ( 'NONE', *, *, #6992, .T. ) ;
#6547 = CARTESIAN_POINT ( 'NONE',  ( 6.851232759387628768, 134.0993825829163200, -14.99999999999999822 ) ) ;
#6548 = ORIENTED_EDGE ( 'NONE', *, *, #1794, .F. ) ;
#6549 = CARTESIAN_POINT ( 'NONE',  ( -80.92353557482439896, 152.5685199100058753, -29.35899209070758786 ) ) ;
#6550 = CARTESIAN_POINT ( 'NONE',  ( 10.76597736162413632, 139.9178931572356532, -11.43282512092270053 ) ) ;
#6551 = ORIENTED_EDGE ( 'NONE', *, *, #9166, .T. ) ;
#6552 = DIRECTION ( 'NONE',  ( -0.000000000000000000, -0.000000000000000000, -1.000000000000000000 ) ) ;
#6553 = CARTESIAN_POINT ( 'NONE',  ( -33.00000000000000711, 171.6227766016838245, 0.000000000000000000 ) ) ;
#6554 = B_SPLINE_CURVE_WITH_KNOTS ( 'NONE', 3,
 ( #15711, #5265, #9247, #6418, #6511, #7656, #13412, #9340, #17310, #13066, #8005, #3859, #10665, #932, #5004, #14478, #14747, #11903, #3590, #10391, #15805, #7733, #11717, #12085, #13240, #2431, #10303, #8983, #13145, #7829, #1196, #6599, #16076, #1111, #14559, #17216, #6322, #13330, #4912, #3683, #11990, #5094, #10487, #2619 ),
 .UNSPECIFIED., .F., .F.,
 ( 4, 2, 2, 2, 2, 2, 2, 2, 2, 2, 2, 2, 2, 2, 2, 2, 2, 2, 2, 2, 2, 4 ),
 ( 0.02539562174428236160, 0.02674754696500278306, 0.02742350957536299205, 0.02809947218572320105, 0.02945139740644361903, 0.03012736001680382456, 0.03080332262716403008, 0.03215524784788444806, 0.03283121045824467787, 0.03350717306860491462, 0.03418313567896515137, 0.03485909828932538118, 0.03621102351004584774, 0.03688698612040607061, 0.03756294873076629348, 0.03891487395148671147, 0.03959083656184691352, 0.04026679917220711558, 0.04161872439292756132, 0.04297064961364800706, 0.04432257483436844586, 0.04702642527580933041 ),
 .UNSPECIFIED. ) ;
#6555 = DIRECTION ( 'NONE',  ( 1.000000000000000000, 0.000000000000000000, -0.000000000000000000 ) ) ;
#6556 = EDGE_CURVE ( 'NONE', #2637, #13756, #1238, .T. ) ;
#6557 = ADVANCED_FACE ( 'NONE', ( #13638 ), #13458, .F. ) ;
#6558 = CARTESIAN_POINT ( 'NONE',  ( -90.80384757729339640, 171.6227766016838245, 0.000000000000000000 ) ) ;
#6559 = CARTESIAN_POINT ( 'NONE',  ( -40.00000000000000000, 4.000000000000000000, 33.00000000000000711 ) ) ;
#6560 = CARTESIAN_POINT ( 'NONE',  ( 49.99999999999998579, 175.6227766016838530, 16.92820660268601429 ) ) ;
#6561 = CYLINDRICAL_SURFACE ( 'NONE', #9516, 30.00000000000000000 ) ;
#6562 = DIRECTION ( 'NONE',  ( 0.000000000000000000, 0.000000000000000000, 1.000000000000000000 ) ) ;
#6563 = CARTESIAN_POINT ( 'NONE',  ( -151.6393416600920716, 171.6227766016838245, 0.000000000000000000 ) ) ;
#6564 = CARTESIAN_POINT ( 'NONE',  ( 28.23642206097335006, 140.8827219813066449, -16.73516917262794479 ) ) ;
#6565 = ORIENTED_EDGE ( 'NONE', *, *, #11863, .F. ) ;
#6566 = CARTESIAN_POINT ( 'NONE',  ( 12.80996511848405994, 130.8496636614418094, -12.93682947221565804 ) ) ;
#6567 = CARTESIAN_POINT ( 'NONE',  ( -13.90980987654335976, 19.99999999999998934, -23.98326992096530219 ) ) ;
#6568 = ORIENTED_EDGE ( 'NONE', *, *, #9372, .T. ) ;
#6569 = DIRECTION ( 'NONE',  ( -1.000000000000000000, -0.000000000000000000, -0.000000000000000000 ) ) ;
#6570 = CARTESIAN_POINT ( 'NONE',  ( -154.9692839938123257, 171.6227766016838245, 0.000000000000000000 ) ) ;
#6571 = VERTEX_POINT ( 'NONE', #9383 ) ;
#6572 = DIRECTION ( 'NONE',  ( 0.000000000000000000, 0.000000000000000000, 1.000000000000000000 ) ) ;
#6573 = CARTESIAN_POINT ( 'NONE',  ( 13.64704021889961361, 139.0043329719002259, 8.527746218697362934 ) ) ;
#6574 = ORIENTED_EDGE ( 'NONE', *, *, #7591, .F. ) ;
#6575 = CARTESIAN_POINT ( 'NONE',  ( -48.00000000000000000, 171.6227766016838245, 0.000000000000000000 ) ) ;
#6576 = VERTEX_POINT ( 'NONE', #13551 ) ;
#6577 = EDGE_CURVE ( 'NONE', #7719, #7374, #11706, .T. ) ;
#6578 = ADVANCED_FACE ( 'NONE', ( #14957 ), #10618, .T. ) ;
#6579 = EDGE_CURVE ( 'NONE', #2548, #14798, #6897, .T. ) ;
#6580 = DIRECTION ( 'NONE',  ( -0.000000000000000000, -0.000000000000000000, 1.000000000000000000 ) ) ;
#6581 = CARTESIAN_POINT ( 'NONE',  ( 30.56347832044301782, 189.1215240515806499, -27.97845313684487678 ) ) ;
#6582 = DIRECTION ( 'NONE',  ( -0.000000000000000000, -1.000000000000000000, 0.000000000000000000 ) ) ;
#6583 = CARTESIAN_POINT ( 'NONE',  ( -16.30611068361414695, 32.76923076921517008, -5.528684565802741702 ) ) ;
#6584 = ORIENTED_EDGE ( 'NONE', *, *, #15063, .F. ) ;
#6585 = SHAPE_REPRESENTATION ( 'socket button head screw_iso_ISO 7380 - M5 x 25 - 25N', ( #3583 ), #14620 ) ;
#6586 = CARTESIAN_POINT ( 'NONE',  ( 49.99999999999998579, 187.6227766016837961, -12.50000337241049309 ) ) ;
#6587 = VERTEX_POINT ( 'NONE', #9636 ) ;
#6588 = CARTESIAN_POINT ( 'NONE',  ( -73.91032892519172037, 192.2167777214562250, -25.78994361341036523 ) ) ;
#6589 = CYLINDRICAL_SURFACE ( 'NONE', #456, 3.999999999999988010 ) ;
#6590 = VERTEX_POINT ( 'NONE', #2915 ) ;
#6591 = ORIENTED_EDGE ( 'NONE', *, *, #13494, .T. ) ;
#6592 = ORIENTED_EDGE ( 'NONE', *, *, #8483, .F. ) ;
#6593 = ADVANCED_FACE ( 'NONE', ( #8303 ), #13717, .F. ) ;
#6594 = CARTESIAN_POINT ( 'NONE',  ( -74.06456496986170635, 151.2142461003564335, -25.93356563065114528 ) ) ;
#6595 = ORIENTED_EDGE ( 'NONE', *, *, #13297, .F. ) ;
#6596 = CARTESIAN_POINT ( 'NONE',  ( 0.000000000000000000, 0.000000000000000000, 0.000000000000000000 ) ) ;
#6597 = CARTESIAN_POINT ( 'NONE',  ( 27.47046887122067105, 138.6908793960143669, -2.448156880351273657 ) ) ;
#6598 = CARTESIAN_POINT ( 'NONE',  ( -17.19488518268993715, 32.09742631896689602, 9.330173263366075886 ) ) ;
#6599 = CARTESIAN_POINT ( 'NONE',  ( 32.79231225559605889, 151.9379092097359205, -28.93992015514735172 ) ) ;
#6600 = CARTESIAN_POINT ( 'NONE',  ( -80.00000000000001421, 196.6227766016838245, -16.00000000000000000 ) ) ;
#6601 = DIRECTION ( 'NONE',  ( -1.000000000000000000, -0.000000000000000000, 0.000000000000000000 ) ) ;
#6602 = VERTEX_POINT ( 'NONE', #17350 ) ;
#6603 = CARTESIAN_POINT ( 'NONE',  ( -80.51989362019833152, 202.6059057426778622, -16.28038605903245539 ) ) ;
#6604 = CARTESIAN_POINT ( 'NONE',  ( 21.04314855419486108, 29.91877537971376455, -12.94423386069545323 ) ) ;
#6605 = CARTESIAN_POINT ( 'NONE',  ( 7.674484246658608733, 133.8653086123773903, 14.91481465347803415 ) ) ;
#6606 = CARTESIAN_POINT ( 'NONE',  ( 34.80468147095351128, 17.99999999999999645, 7.619145204522578041 ) ) ;
#6607 = CARTESIAN_POINT ( 'NONE',  ( -35.49999999999998579, 10.00000000000000178, -28.00000000000000355 ) ) ;
#6608 = EDGE_LOOP ( 'NONE', ( #17484, #4057, #15015 ) ) ;
#6609 = CARTESIAN_POINT ( 'NONE',  ( -85.89213624354479748, 141.9593924407984957, -14.48320912595414711 ) ) ;
#6610 = DIRECTION ( 'NONE',  ( 0.000000000000000000, 0.000000000000000000, 1.000000000000000000 ) ) ;
#6611 = CARTESIAN_POINT ( 'NONE',  ( 34.46640061674913369, 198.8884873102157655, 18.59522663992144942 ) ) ;
#6612 = EDGE_CURVE ( 'NONE', #14270, #7418, #17146, .T. ) ;
#6613 = ORIENTED_EDGE ( 'NONE', *, *, #5218, .T. ) ;
#6614 = EDGE_CURVE ( 'NONE', #2922, #16329, #9514, .T. ) ;
#6615 = DIRECTION ( 'NONE',  ( -1.000000000000000000, 0.000000000000000000, 8.673617379884037937E-17 ) ) ;
#6616 = DIRECTION ( 'NONE',  ( -0.08715574274764831264, 0.9961946980917464334, 0.000000000000000000 ) ) ;
#6617 = ORIENTED_EDGE ( 'NONE', *, *, #14467, .T. ) ;
#6618 =( LENGTH_UNIT ( ) NAMED_UNIT ( * ) SI_UNIT ( .MILLI., .METRE. ) );
#6619 = CARTESIAN_POINT ( 'NONE',  ( -80.00000000000001421, 196.6227766016838245, 10.00000000000000178 ) ) ;
#6620 = CARTESIAN_POINT ( 'NONE',  ( 50.00000000000000000, 171.6227766016838245, 0.000000000000000000 ) ) ;
#6621 = AXIS2_PLACEMENT_3D ( 'NONE', #5295, #10857, #9438 ) ;
#6622 = CARTESIAN_POINT ( 'NONE',  ( -85.34448289831571799, 143.8733932267928424, -21.33602313251873639 ) ) ;
#6623 = ADVANCED_FACE ( 'NONE', ( #13817, #13907 ), #7163, .T. ) ;
#6624 = CARTESIAN_POINT ( 'NONE',  ( -25.81010901361623056, 20.00000000000000000, 13.97188021846430850 ) ) ;
#6625 = EDGE_CURVE ( 'NONE', #15082, #11068, #11771, .T. ) ;
#6626 = ORIENTED_EDGE ( 'NONE', *, *, #14861, .T. ) ;
#6627 = CARTESIAN_POINT ( 'NONE',  ( 49.99999999999998579, 159.6227766016838814, -5.571800142134975431 ) ) ;
#6628 = LINE ( 'NONE', #11930, #10435 ) ;
#6629 = DIRECTION ( 'NONE',  ( -1.000000000000000000, 0.000000000000000000, 0.000000000000000000 ) ) ;
#6630 = PLANE ( 'NONE',  #13148 ) ;
#6631 = ORIENTED_EDGE ( 'NONE', *, *, #2081, .T. ) ;
#6632 = AXIS2_PLACEMENT_3D ( 'NONE', #16759, #10003, #7183 ) ;
#6633 = LINE ( 'NONE', #3718, #6151 ) ;
#6634 = AXIS2_PLACEMENT_3D ( 'NONE', #5968, #15679, #12857 ) ;
#6635 = ORIENTED_EDGE ( 'NONE', *, *, #14345, .T. ) ;
#6636 = CARTESIAN_POINT ( 'NONE',  ( -85.86161444987101277, 147.9152928535322928, -25.74888847741385689 ) ) ;
#6637 = CARTESIAN_POINT ( 'NONE',  ( 16.61152767523464391, 142.9573811237880534, -16.36000751420521837 ) ) ;
#6638 = VERTEX_POINT ( 'NONE', #8574 ) ;
#6639 = CARTESIAN_POINT ( 'NONE',  ( -187.6513770290094669, 172.4976050944027008, 2.196701325097758950 ) ) ;
#6640 = CARTESIAN_POINT ( 'NONE',  ( -32.14917720409452073, 119.8847850876509966, -5.472305571547330771 ) ) ;
#6641 = CARTESIAN_POINT ( 'NONE',  ( -50.00000000000000000, 171.6227766016838245, 0.000000000000000000 ) ) ;
#6642 = DIRECTION ( 'NONE',  ( -0.000000000000000000, -0.000000000000000000, -1.000000000000000000 ) ) ;
#6643 = DIRECTION ( 'NONE',  ( 0.000000000000000000, 0.000000000000000000, -1.000000000000000000 ) ) ;
#6644 = ADVANCED_FACE ( 'NONE', ( #426, #12748 ), #1939, .T. ) ;
#6645 = CIRCLE ( 'NONE', #8879, 12.00000000000000000 ) ;
#6646 = CARTESIAN_POINT ( 'NONE',  ( 22.25017171248248005, 17.99999999999544542, -8.611421531743401303 ) ) ;
#6647 = FACE_OUTER_BOUND ( 'NONE', #3013, .T. ) ;
#6648 = FACE_OUTER_BOUND ( 'NONE', #4985, .T. ) ;
#6649 = VECTOR ( 'NONE', #14445, 1000.000000000000000 ) ;
#6650 = DIRECTION ( 'NONE',  ( 1.000000000000000000, 0.000000000000000000, 0.000000000000000000 ) ) ;
#6651 = CARTESIAN_POINT ( 'NONE',  ( 196.0000000000000000, 187.6227766016837961, -12.50000337241049309 ) ) ;
#6652 = ORIENTED_EDGE ( 'NONE', *, *, #15549, .F. ) ;
#6653 = CARTESIAN_POINT ( 'NONE',  ( 17.39133856982844506, 125.9242906883583970, -6.521754810248964418 ) ) ;
#6654 = ORIENTED_EDGE ( 'NONE', *, *, #1160, .F. ) ;
#6655 = DIRECTION ( 'NONE',  ( 1.000000000000000000, 0.000000000000000000, -0.000000000000000000 ) ) ;
#6656 = DIRECTION ( 'NONE',  ( 1.000000000000000000, -0.000000000000000000, -0.000000000000000000 ) ) ;
#6657 = EDGE_CURVE ( 'NONE', #3217, #6998, #3308, .T. ) ;
#6658 = VERTEX_POINT ( 'NONE', #15387 ) ;
#6659 = CARTESIAN_POINT ( 'NONE',  ( -14.55266450408011636, 19.99999999999999645, 23.76398220081675206 ) ) ;
#6660 = CARTESIAN_POINT ( 'NONE',  ( 14.80221254542069076, 126.7206120434983490, 7.900896541359456293 ) ) ;
#6661 = AXIS2_PLACEMENT_3D ( 'NONE', #14349, #6286, #17086 ) ;
#6662 = VERTEX_POINT ( 'NONE', #11058 ) ;
#6663 = CARTESIAN_POINT ( 'NONE',  ( 17.04141343047935564, 29.97166846511136029, 14.77658840773744409 ) ) ;
#6664 = CIRCLE ( 'NONE', #14021, 3.999999999999985789 ) ;
#6665 = VERTEX_POINT ( 'NONE', #4603 ) ;
#6666 = CARTESIAN_POINT ( 'NONE',  ( -95.00000000000000000, 143.9321776784423150, 5.086680500673126297E-15 ) ) ;
#6667 = DIRECTION ( 'NONE',  ( 0.000000000000000000, 0.000000000000000000, -1.000000000000000000 ) ) ;
#6668 = CARTESIAN_POINT ( 'NONE',  ( 196.0000000000000000, 159.6227766016838814, -3.071800142134975431 ) ) ;
#6669 = CARTESIAN_POINT ( 'NONE',  ( -11.82448321327245466, 31.42688426858654438, -11.97038274549936254 ) ) ;
#6670 = PRESENTATION_LAYER_ASSIGNMENT (  '', '', ( #3546 ) ) ;
#6671 = VERTEX_POINT ( 'NONE', #9722 ) ;
#6672 = CARTESIAN_POINT ( 'NONE',  ( 32.56480294350151183, 150.9309764409412367, 25.70786830908634002 ) ) ;
#6673 = VECTOR ( 'NONE', #16260, 1000.000000000000000 ) ;
#6674 = ORIENTED_EDGE ( 'NONE', *, *, #5445, .T. ) ;
#6675 = DIRECTION ( 'NONE',  ( 0.000000000000000000, -0.8660254037844413721, -0.4999999999999953371 ) ) ;
#6676 = CARTESIAN_POINT ( 'NONE',  ( 39.99999999999998579, 20.00000000000000000, -30.00000000000001066 ) ) ;
#6677 = EDGE_CURVE ( 'NONE', #12789, #13912, #8102, .T. ) ;
#6678 = ORIENTED_EDGE ( 'NONE', *, *, #2398, .F. ) ;
#6679 = EDGE_CURVE ( 'NONE', #4216, #5512, #4517, .T. ) ;
#6680 = AXIS2_PLACEMENT_3D ( 'NONE', #3280, #8686, #14092 ) ;
#6681 = ORIENTED_EDGE ( 'NONE', *, *, #13254, .F. ) ;
#6682 = EDGE_CURVE ( 'NONE', #14903, #15136, #9816, .T. ) ;
#6683 = ORIENTED_EDGE ( 'NONE', *, *, #3593, .F. ) ;
#6684 = AXIS2_PLACEMENT_3D ( 'NONE', #6487, #2323, #3565 ) ;
#6685 = ORIENTED_EDGE ( 'NONE', *, *, #1424, .T. ) ;
#6686 = PRODUCT_CONTEXT ( 'NONE', #7328, 'mechanical' ) ;
#6687 = CARTESIAN_POINT ( 'NONE',  ( -40.00000000000000000, 0.000000000000000000, 33.00000000000000711 ) ) ;
#6688 = AXIS2_PLACEMENT_3D ( 'NONE', #14813, #2610, #17116 ) ;
#6689 = DIRECTION ( 'NONE',  ( 1.000000000000000000, 0.000000000000000000, -0.000000000000000000 ) ) ;
#6690 = DIRECTION ( 'NONE',  ( -0.000000000000000000, -0.000000000000000000, -1.000000000000000000 ) ) ;
#6691 = DIRECTION ( 'NONE',  ( 0.000000000000000000, 0.000000000000000000, 1.000000000000000000 ) ) ;
#6692 = DIRECTION ( 'NONE',  ( -1.000000000000000000, 0.000000000000000000, 0.000000000000000000 ) ) ;
#6693 = EDGE_LOOP ( 'NONE', ( #16160, #11336, #8290, #3152 ) ) ;
#6694 = DIRECTION ( 'NONE',  ( 1.000000000000000000, 0.000000000000000000, -0.000000000000000000 ) ) ;
#6695 = DIRECTION ( 'NONE',  ( 1.000000000000000000, 0.000000000000000000, 0.000000000000000000 ) ) ;
#6696 = FACE_OUTER_BOUND ( 'NONE', #11583, .T. ) ;
#6697 = CARTESIAN_POINT ( 'NONE',  ( 29.98123639043839006, 18.00000000000000000, 18.19121573219640098 ) ) ;
#6698 = FACE_OUTER_BOUND ( 'NONE', #11720, .T. ) ;
#6699 = EDGE_LOOP ( 'NONE', ( #11829, #13069, #8413, #2492 ) ) ;
#6700 = DIRECTION ( 'NONE',  ( 0.8660254037844378194, -0.5000000000000015543, -0.000000000000000000 ) ) ;
#6701 = CIRCLE ( 'NONE', #3873, 1.500000000000000000 ) ;
#6702 = AXIS2_PLACEMENT_3D ( 'NONE', #9657, #1261, #8326 ) ;
#6703 = CIRCLE ( 'NONE', #12064, 740.0000000000000000 ) ;
#6704 = VECTOR ( 'NONE', #11484, 1000.000000000000000 ) ;
#6705 = DIRECTION ( 'NONE',  ( -0.000000000000000000, -0.000000000000000000, -1.000000000000000000 ) ) ;
#6706 = CARTESIAN_POINT ( 'NONE',  ( -151.0000000000000284, 171.6227766016838245, -6.000000000000005329 ) ) ;
#6707 = ORIENTED_EDGE ( 'NONE', *, *, #14410, .F. ) ;
#6708 = CARTESIAN_POINT ( 'NONE',  ( 2.950000000000001066, 0.000000000000000000, 2.699999999999999289 ) ) ;
#6709 = VERTEX_POINT ( 'NONE', #7343 ) ;
#6710 = DIRECTION ( 'NONE',  ( -0.000000000000000000, -1.000000000000000000, 2.312964634635742267E-15 ) ) ;
#6711 = FACE_BOUND ( 'NONE', #9913, .T. ) ;
#6712 = CARTESIAN_POINT ( 'NONE',  ( -78.22549311270449834, 140.8861252344925106, -16.74142298344136393 ) ) ;
#6713 = AXIS2_PLACEMENT_3D ( 'NONE', #16993, #8670, #7423 ) ;
#6714 = AXIS2_PLACEMENT_3D ( 'NONE', #13063, #11987, #17122 ) ;
#6715 = CARTESIAN_POINT ( 'NONE',  ( -21.35874126517689930, 20.00000000000000000, 19.71585776365618869 ) ) ;
#6716 = VECTOR ( 'NONE', #16452, 1000.000000000000000 ) ;
#6717 = ORIENTED_EDGE ( 'NONE', *, *, #16182, .F. ) ;
#6718 = DIRECTION ( 'NONE',  ( -1.000000000000000000, 0.000000000000000000, 0.000000000000000000 ) ) ;
#6719 = CARTESIAN_POINT ( 'NONE',  ( -72.50000000000000000, 196.6227766016838245, -13.00000000000000000 ) ) ;
#6720 = DIRECTION ( 'NONE',  ( 1.000000000000000000, 0.000000000000000000, 0.000000000000000000 ) ) ;
#6721 = EDGE_CURVE ( 'NONE', #4462, #15051, #16554, .T. ) ;
#6722 = CARTESIAN_POINT ( 'NONE',  ( 225.0000000000000000, 89.99999999999997158, -15.00000000000000000 ) ) ;
#6723 = ORIENTED_EDGE ( 'NONE', *, *, #12848, .T. ) ;
#6724 = CARTESIAN_POINT ( 'NONE',  ( 16.34705933256690713, 136.9208395216682561, -6.505922558274787271 ) ) ;
#6725 = CIRCLE ( 'NONE', #10674, 1.500000000000000000 ) ;
#6726 = ORIENTED_EDGE ( 'NONE', *, *, #9353, .F. ) ;
#6727 = CARTESIAN_POINT ( 'NONE',  ( -33.00000000000000711, 171.6227766016838245, 5.000000000000007994 ) ) ;
#6728 = VECTOR ( 'NONE', #4723, 1000.000000000000000 ) ;
#6729 = CARTESIAN_POINT ( 'NONE',  ( 14.12560798726494760, 138.8049619564753243, -7.597757983846324947 ) ) ;
#6730 = VERTEX_POINT ( 'NONE', #7083 ) ;
#6731 = DIRECTION ( 'NONE',  ( 0.000000000000000000, 0.000000000000000000, 1.000000000000000000 ) ) ;
#6732 = DIRECTION ( 'NONE',  ( 0.000000000000000000, 0.000000000000000000, -1.000000000000000000 ) ) ;
#6733 = DIRECTION ( 'NONE',  ( -1.000000000000000000, 0.000000000000000000, 0.000000000000000000 ) ) ;
#6734 = CARTESIAN_POINT ( 'NONE',  ( 30.00000000000001066, 146.6227766016838245, 1.387778780781445676E-14 ) ) ;
#6735 = CARTESIAN_POINT ( 'NONE',  ( 16.25302816831168329, 18.00000000000000000, -25.00000000000000000 ) ) ;
#6736 = CARTESIAN_POINT ( 'NONE',  ( 22.51491806150639974, 29.85019096660411364, -7.572044396946283840 ) ) ;
#6737 = LINE ( 'NONE', #90, #2757 ) ;
#6738 = FACE_OUTER_BOUND ( 'NONE', #13787, .T. ) ;
#6739 = AXIS2_PLACEMENT_3D ( 'NONE', #7045, #4567, #8719 ) ;
#6740 = DIRECTION ( 'NONE',  ( 1.000000000000000000, 0.000000000000000000, 0.000000000000000000 ) ) ;
#6741 = EDGE_CURVE ( 'NONE', #4376, #10086, #13978, .T. ) ;
#6742 = AXIS2_PLACEMENT_3D ( 'NONE', #9720, #85, #2830 ) ;
#6743 = COLOUR_RGB ( '', 0.72549020, 0.75294118, 0.79215686) ;
#6744 = CARTESIAN_POINT ( 'NONE',  ( -48.00000000000000000, 171.6227766016838245, 0.000000000000000000 ) ) ;
#6745 = ORIENTED_EDGE ( 'NONE', *, *, #305, .T. ) ;
#6746 = CARTESIAN_POINT ( 'NONE',  ( 14.34366722128227067, 129.4994645064758174, -11.74322308516846647 ) ) ;
#6747 = VERTEX_POINT ( 'NONE', #3360 ) ;
#6748 = DIRECTION ( 'NONE',  ( -1.000000000000000000, -0.000000000000000000, -0.000000000000000000 ) ) ;
#6749 = ADVANCED_FACE ( 'NONE', ( #5934 ), #8756, .F. ) ;
#6750 = LINE ( 'NONE', #1604, #4143 ) ;
#6751 = ORIENTED_EDGE ( 'NONE', *, *, #8084, .F. ) ;
#6752 = EDGE_CURVE ( 'NONE', #10662, #8295, #8594, .T. ) ;
#6753 = CARTESIAN_POINT ( 'NONE',  ( -12.78554710720352894, 31.18907022382790117, 13.71297843187037202 ) ) ;
#6754 = EDGE_CURVE ( 'NONE', #16058, #3029, #6012, .T. ) ;
#6755 = CARTESIAN_POINT ( 'NONE',  ( 18.30724418481818461, 142.5286147297794344, 15.57621362570774437 ) ) ;
#6756 = VERTEX_POINT ( 'NONE', #3264 ) ;
#6757 = VECTOR ( 'NONE', #9466, 1000.000000000000000 ) ;
#6758 = CARTESIAN_POINT ( 'NONE',  ( 14.93242934743710393, 30.00000000000000000, -13.00000000000000178 ) ) ;
#6759 = CIRCLE ( 'NONE', #16655, 6.000000000000005329 ) ;
#6760 = ORIENTED_EDGE ( 'NONE', *, *, #14312, .T. ) ;
#6761 = DIRECTION ( 'NONE',  ( 1.000000000000000000, 0.000000000000000000, 0.000000000000000000 ) ) ;
#6762 = CARTESIAN_POINT ( 'NONE',  ( 37.46328901163953162, 195.8564978660714360, -22.40111672564487222 ) ) ;
#6763 = FACE_OUTER_BOUND ( 'NONE', #3564, .T. ) ;
#6764 = ADVANCED_FACE ( 'NONE', ( #8494 ), #2375, .T. ) ;
#6765 = CARTESIAN_POINT ( 'NONE',  ( -22.99999999999999645, 100.0000000000000142, -15.00000000000000000 ) ) ;
#6766 = ORIENTED_EDGE ( 'NONE', *, *, #625, .F. ) ;
#6767 = CARTESIAN_POINT ( 'NONE',  ( 29.59441769460779526, 151.6102025845143828, 26.23924109008940420 ) ) ;
#6768 = AXIS2_PLACEMENT_3D ( 'NONE', #4779, #6272, #15573 ) ;
#6769 = CIRCLE ( 'NONE', #15801, 10.00000000000000000 ) ;
#6770 = ORIENTED_EDGE ( 'NONE', *, *, #9337, .T. ) ;
#6771 = CARTESIAN_POINT ( 'NONE',  ( -84.88846745512550740, 190.9286879163519757, -26.76420670456570505 ) ) ;
#6772 = CIRCLE ( 'NONE', #2232, 2.499999999999998668 ) ;
#6773 = CYLINDRICAL_SURFACE ( 'NONE', #2151, 2.500000000000002220 ) ;
#6774 = VERTEX_POINT ( 'NONE', #15119 ) ;
#6775 = VERTEX_POINT ( 'NONE', #12653 ) ;
#6776 = VERTEX_POINT ( 'NONE', #14079 ) ;
#6777 = CARTESIAN_POINT ( 'NONE',  ( 13.53786153804125725, 141.8544345782132439, 18.40805394434863018 ) ) ;
#6778 = CIRCLE ( 'NONE', #16400, 2.500000000000002220 ) ;
#6779 = ORIENTED_EDGE ( 'NONE', *, *, #15701, .T. ) ;
#6780 = ITEM_DEFINED_TRANSFORMATION ( 'NONE', 'NONE', #5861,  #3583 ) ;
#6781 = VECTOR ( 'NONE', #15772, 1000.000000000000114 ) ;
#6782 = CYLINDRICAL_SURFACE ( 'NONE', #7090, 20.00000000000000355 ) ;
#6783 = AXIS2_PLACEMENT_3D ( 'NONE', #17083, #809, #2213 ) ;
#6784 = FACE_OUTER_BOUND ( 'NONE', #14962, .T. ) ;
#6785 = CARTESIAN_POINT ( 'NONE',  ( -80.00000000000001421, 196.6227766016838245, -35.00200000000000244 ) ) ;
#6786 = EDGE_CURVE ( 'NONE', #2211, #735, #3002, .T. ) ;
#6787 = LINE ( 'NONE', #12348, #3147 ) ;
#6788 = EDGE_CURVE ( 'NONE', #9434, #14250, #13005, .T. ) ;
#6789 = LINE ( 'NONE', #8186, #13162 ) ;
#6790 = ADVANCED_FACE ( 'NONE', ( #13172 ), #12823, .F. ) ;
#6791 = ORIENTED_EDGE ( 'NONE', *, *, #2, .T. ) ;
#6792 = CARTESIAN_POINT ( 'NONE',  ( -81.03644165218622675, 202.5339273643435547, -16.41656018636075132 ) ) ;
#6793 = LINE ( 'NONE', #3868, #7077 ) ;
#6794 = CARTESIAN_POINT ( 'NONE',  ( 22.61491075001043782, 18.00000000000000000, 23.50024419593056635 ) ) ;
#6795 = CARTESIAN_POINT ( 'NONE',  ( 196.0000000000000000, 175.6227766016838530, 16.92820660268601429 ) ) ;
#6796 = DIRECTION ( 'NONE',  ( -0.000000000000000000, -0.000000000000000000, -1.000000000000000000 ) ) ;
#6797 = CIRCLE ( 'NONE', #3677, 10.00000000000000178 ) ;
#6798 = VECTOR ( 'NONE', #8834, 1000.000000000000000 ) ;
#6799 = DIRECTION ( 'NONE',  ( 0.000000000000000000, 0.000000000000000000, -1.000000000000000000 ) ) ;
#6800 = ORIENTED_EDGE ( 'NONE', *, *, #10599, .T. ) ;
#6801 = DIRECTION ( 'NONE',  ( -1.000000000000000000, -0.000000000000000000, -0.000000000000000000 ) ) ;
#6802 = ORIENTED_EDGE ( 'NONE', *, *, #8168, .T. ) ;
#6803 = DIRECTION ( 'NONE',  ( -1.000000000000000000, -0.000000000000000000, -0.000000000000000000 ) ) ;
#6804 = VECTOR ( 'NONE', #16263, 1000.000000000000000 ) ;
#6805 = DIRECTION ( 'NONE',  ( 0.000000000000000000, -0.8660254037844413721, 0.4999999999999953371 ) ) ;
#6806 = AXIS2_PLACEMENT_3D ( 'NONE', #5372, #5795, #1812 ) ;
#6807 = EDGE_CURVE ( 'NONE', #7959, #13616, #5493, .T. ) ;
#6808 = EDGE_CURVE ( 'NONE', #2922, #15641, #8324, .T. ) ;
#6809 = CARTESIAN_POINT ( 'NONE',  ( -11.98734322101357641, 20.00000000000000000, 24.50584837321703802 ) ) ;
#6810 = ORIENTED_EDGE ( 'NONE', *, *, #5092, .T. ) ;
#6811 = FACE_OUTER_BOUND ( 'NONE', #11939, .T. ) ;
#6812 = DIRECTION ( 'NONE',  ( -0.000000000000000000, -0.000000000000000000, -1.000000000000000000 ) ) ;
#6813 = CARTESIAN_POINT ( 'NONE',  ( -3.000000000000000888, 171.6227766016838245, 0.000000000000000000 ) ) ;
#6814 = DIRECTION ( 'NONE',  ( -0.000000000000000000, -0.000000000000000000, 1.000000000000000000 ) ) ;
#6815 = VECTOR ( 'NONE', #8541, 1000.000000000000000 ) ;
#6816 = CARTESIAN_POINT ( 'NONE',  ( 14.18611645313626290, 129.6406627243902676, -11.87032202561248617 ) ) ;
#6817 = ORIENTED_EDGE ( 'NONE', *, *, #4625, .T. ) ;
#6818 = CARTESIAN_POINT ( 'NONE',  ( -27.99999999999998224, 10.00000000000000000, -30.00000000000000355 ) ) ;
#6819 = AXIS2_PLACEMENT_3D ( 'NONE', #11362, #10349, #3042 ) ;
#6820 = CARTESIAN_POINT ( 'NONE',  ( 196.0000000000000000, 171.6227766016838245, -15.00000337241049131 ) ) ;
#6821 = EDGE_LOOP ( 'NONE', ( #9192, #1496, #16498, #3716 ) ) ;
#6822 = LINE ( 'NONE', #13634, #3108 ) ;
#6823 = EDGE_CURVE ( 'NONE', #11878, #102, #14420, .T. ) ;
#6824 = CARTESIAN_POINT ( 'NONE',  ( 27.93429729575420950, 192.0656250386302872, 25.90562197801993349 ) ) ;
#6825 = CARTESIAN_POINT ( 'NONE',  ( 32.29638371061065527, 18.00000000000000000, -15.01265034258821096 ) ) ;
#6826 = CARTESIAN_POINT ( 'NONE',  ( 30.80964797964692536, 18.00000000000000000, -17.18170494867161224 ) ) ;
#6827 = DIRECTION ( 'NONE',  ( -0.000000000000000000, -0.000000000000000000, -1.000000000000000000 ) ) ;
#6828 = CIRCLE ( 'NONE', #11344, 2.500000000000002220 ) ;
#6829 = DIRECTION ( 'NONE',  ( -0.000000000000000000, -0.000000000000000000, -1.000000000000000000 ) ) ;
#6830 = DIRECTION ( 'NONE',  ( 0.000000000000000000, 0.000000000000000000, 1.000000000000000000 ) ) ;
#6831 = CARTESIAN_POINT ( 'NONE',  ( 24.00000000000000711, 146.2509476181506329, -24.11540106065089262 ) ) ;
#6832 = VERTEX_POINT ( 'NONE', #11741 ) ;
#6833 = FACE_OUTER_BOUND ( 'NONE', #14839, .T. ) ;
#6834 = EDGE_LOOP ( 'NONE', ( #16175, #10831 ) ) ;
#6835 = DIRECTION ( 'NONE',  ( 0.000000000000000000, 0.000000000000000000, 1.000000000000000000 ) ) ;
#6836 = LINE ( 'NONE', #3011, #1602 ) ;
#6837 = ORIENTED_EDGE ( 'NONE', *, *, #15532, .F. ) ;
#6838 = CARTESIAN_POINT ( 'NONE',  ( 22.93524650466160963, 29.84210526315773748, -4.999999999999999112 ) ) ;
#6839 = DIRECTION ( 'NONE',  ( -0.000000000000000000, -0.000000000000000000, 1.000000000000000000 ) ) ;
#6840 = VECTOR ( 'NONE', #1709, 1000.000000000000000 ) ;
#6841 = ORIENTED_EDGE ( 'NONE', *, *, #1031, .F. ) ;
#6842 = CARTESIAN_POINT ( 'NONE',  ( 22.53671098836050746, 147.3890553372962700, -22.40111672564484024 ) ) ;
#6843 = EDGE_CURVE ( 'NONE', #10402, #2789, #11424, .T. ) ;
#6844 = ORIENTED_EDGE ( 'NONE', *, *, #10609, .F. ) ;
#6845 = CARTESIAN_POINT ( 'NONE',  ( -90.80384757729339640, 204.6227766016838245, 0.000000000000000000 ) ) ;
#6846 = CARTESIAN_POINT ( 'NONE',  ( -725.0000000000000000, 19.99999999999995737, 0.000000000000000000 ) ) ;
#6847 = DIRECTION ( 'NONE',  ( -0.08715574274764831264, 0.9961946980917464334, 0.000000000000000000 ) ) ;
#6848 = VERTEX_POINT ( 'NONE', #2285 ) ;
#6849 = LINE ( 'NONE', #6765, #12858 ) ;
#6850 = EDGE_CURVE ( 'NONE', #12878, #1164, #2664, .T. ) ;
#6851 = EDGE_CURVE ( 'NONE', #9797, #4327, #15737, .T. ) ;
#6852 = ORIENTED_EDGE ( 'NONE', *, *, #2678, .T. ) ;
#6853 = DIRECTION ( 'NONE',  ( -1.000000000000000000, -0.000000000000000000, -0.000000000000000000 ) ) ;
#6854 = ORIENTED_EDGE ( 'NONE', *, *, #10790, .T. ) ;
#6855 = CARTESIAN_POINT ( 'NONE',  ( -86.47240542152535170, 192.8264746069454816, -25.28784208911848808 ) ) ;
#6856 = CARTESIAN_POINT ( 'NONE',  ( -100.0000000000000000, 171.6227766016838245, 0.000000000000000000 ) ) ;
#6857 = DIRECTION ( 'NONE',  ( 1.000000000000000000, -0.000000000000000000, -0.000000000000000000 ) ) ;
#6858 = EDGE_LOOP ( 'NONE', ( #3396, #6069, #8709, #3848 ) ) ;
#6859 = EDGE_LOOP ( 'NONE', ( #8165, #16787 ) ) ;
#6860 = CARTESIAN_POINT ( 'NONE',  ( 13.85534145189689248, 141.7971685630157879, 18.31519266891907094 ) ) ;
#6861 = VERTEX_POINT ( 'NONE', #2367 ) ;
#6862 = APPLICATION_PROTOCOL_DEFINITION ( 'draft international standard', 'automotive_design', 1998, #5286 ) ;
#6863 = DIRECTION ( 'NONE',  ( 0.000000000000000000, 0.000000000000000000, -1.000000000000000000 ) ) ;
#6864 = PLANE ( 'NONE',  #3558 ) ;
#6865 = CARTESIAN_POINT ( 'NONE',  ( 30.00000000000000355, 196.6227766016838245, 35.00200000000000244 ) ) ;
#6866 = LINE ( 'NONE', #4120, #11604 ) ;
#6867 = CARTESIAN_POINT ( 'NONE',  ( -75.00000000000002842, 146.6227766016838245, 0.000000000000000000 ) ) ;
#6868 = ORIENTED_EDGE ( 'NONE', *, *, #2877, .F. ) ;
#6869 = CARTESIAN_POINT ( 'NONE',  ( -77.02080656390279501, 201.8349995435116568, -17.67084604013262350 ) ) ;
#6870 = CARTESIAN_POINT ( 'NONE',  ( 48.00000000000000711, 155.6227766016839098, 12.50000337241049309 ) ) ;
#6871 = CARTESIAN_POINT ( 'NONE',  ( -25.00000000000002132, 120.0000000000000284, 5.000000000000023093 ) ) ;
#6872 = LINE ( 'NONE', #6795, #3352 ) ;
#6873 = DIRECTION ( 'NONE',  ( -0.000000000000000000, -0.000000000000000000, -1.000000000000000000 ) ) ;
#6874 = VERTEX_POINT ( 'NONE', #7592 ) ;
#6875 = CARTESIAN_POINT ( 'NONE',  ( -90.80384757729339640, 138.6227766016838245, 0.000000000000000000 ) ) ;
#6876 = EDGE_CURVE ( 'NONE', #7826, #12193, #3231, .T. ) ;
#6877 = ORIENTED_EDGE ( 'NONE', *, *, #8003, .T. ) ;
#6878 = ORIENTED_EDGE ( 'NONE', *, *, #1599, .F. ) ;
#6879 = CARTESIAN_POINT ( 'NONE',  ( -84.88882470713647876, 145.4280468792801742, 20.09168135694114454 ) ) ;
#6880 = DIRECTION ( 'NONE',  ( 1.000000000000000000, 0.000000000000000000, 0.000000000000000000 ) ) ;
#6881 = VERTEX_POINT ( 'NONE', #14240 ) ;
#6882 = CARTESIAN_POINT ( 'NONE',  ( -38.00000000000000000, 20.00000000000000000, 28.00000000000000355 ) ) ;
#6883 = DIRECTION ( 'NONE',  ( 0.000000000000000000, -1.000000000000000000, 0.000000000000000000 ) ) ;
#6884 = DIRECTION ( 'NONE',  ( -1.000000000000000000, -0.000000000000000000, -0.000000000000000000 ) ) ;
#6885 = SURFACE_STYLE_FILL_AREA ( #5563 ) ;
#6886 = CARTESIAN_POINT ( 'NONE',  ( 15.80099858973940030, 127.9994182179736413, -10.08996921773076316 ) ) ;
#6887 = EDGE_CURVE ( 'NONE', #14780, #539, #14817, .T. ) ;
#6888 = ADVANCED_FACE ( 'NONE', ( #10325 ), #14498, .F. ) ;
#6889 = ADVANCED_FACE ( 'NONE', ( #5119 ), #2103, .F. ) ;
#6890 = ORIENTED_EDGE ( 'NONE', *, *, #7068, .T. ) ;
#6891 = DIRECTION ( 'NONE',  ( 1.000000000000000000, 0.000000000000000000, 0.000000000000000000 ) ) ;
#6892 = EDGE_LOOP ( 'NONE', ( #7050, #8057 ) ) ;
#6893 = DIRECTION ( 'NONE',  ( 0.000000000000000000, 0.000000000000000000, 1.000000000000000000 ) ) ;
#6894 = DIRECTION ( 'NONE',  ( -1.000000000000000000, -0.000000000000000000, 0.000000000000000000 ) ) ;
#6895 = CARTESIAN_POINT ( 'NONE',  ( 2.370000000000000551, 0.000000000000000000, 0.000000000000000000 ) ) ;
#6896 = CARTESIAN_POINT ( 'NONE',  ( -103.0000000000000142, 171.6227766016838245, 0.000000000000000000 ) ) ;
#6897 = LINE ( 'NONE', #170, #2740 ) ;
#6898 = DIRECTION ( 'NONE',  ( -1.000000000000000000, -0.000000000000000000, 0.000000000000000000 ) ) ;
#6899 = CARTESIAN_POINT ( 'NONE',  ( 22.73104287435775461, 29.84603067649059227, 6.814483377121257845 ) ) ;
#6900 = CARTESIAN_POINT ( 'NONE',  ( 14.93242934743711992, 18.00000000000000355, -25.00000000000000000 ) ) ;
#6901 = AXIS2_PLACEMENT_3D ( 'NONE', #7758, #11835, #6182 ) ;
#6902 = EDGE_LOOP ( 'NONE', ( #8997, #16012, #6723, #4114 ) ) ;
#6903 = CARTESIAN_POINT ( 'NONE',  ( -10.04118010627649049, 19.99999999999999645, -24.87462214923097648 ) ) ;
#6904 = VECTOR ( 'NONE', #3477, 1000.000000000000000 ) ;
#6905 = ORIENTED_EDGE ( 'NONE', *, *, #10186, .T. ) ;
#6906 = DIRECTION ( 'NONE',  ( 0.000000000000000000, 1.000000000000000000, 0.000000000000000000 ) ) ;
#6907 = FACE_OUTER_BOUND ( 'NONE', #2551, .T. ) ;
#6908 = ORIENTED_EDGE ( 'NONE', *, *, #16040, .F. ) ;
#6909 = CARTESIAN_POINT ( 'NONE',  ( -14.51002702888200702, 31.55035369552022928, 12.57309263104575869 ) ) ;
#6910 = CARTESIAN_POINT ( 'NONE',  ( -18.25212770525996930, 32.30769230769230660, 0.000000000000000000 ) ) ;
#6911 = ORIENTED_EDGE ( 'NONE', *, *, #14421, .F. ) ;
#6912 = CARTESIAN_POINT ( 'NONE',  ( 36.47240542152533749, 150.4190785964221675, -25.28784208911848808 ) ) ;
#6913 = CIRCLE ( 'NONE', #4929, 239.9999999999999716 ) ;
#6914 = VERTEX_POINT ( 'NONE', #8026 ) ;
#6915 = CIRCLE ( 'NONE', #2963, 2.500000000000002220 ) ;
#6916 = LINE ( 'NONE', #14727, #15721 ) ;
#6917 = CARTESIAN_POINT ( 'NONE',  ( 36.08967107480828673, 192.2167777214563102, -25.78994361341037944 ) ) ;
#6918 = LINE ( 'NONE', #11158, #16172 ) ;
#6919 = VERTEX_POINT ( 'NONE', #8116 ) ;
#6920 = DIRECTION ( 'NONE',  ( 0.000000000000000000, 0.000000000000000000, -1.000000000000000000 ) ) ;
#6921 = ORIENTED_EDGE ( 'NONE', *, *, #17138, .F. ) ;
#6922 = CARTESIAN_POINT ( 'NONE',  ( 29.79050797247102977, 151.6222428389254731, 26.24840280143448012 ) ) ;
#6923 = EDGE_CURVE ( 'NONE', #2095, #2500, #10593, .T. ) ;
#6924 = EDGE_LOOP ( 'NONE', ( #7855, #8965, #1374, #507 ) ) ;
#6925 = ADVANCED_FACE ( 'NONE', ( #13529 ), #4061, .T. ) ;
#6926 = CARTESIAN_POINT ( 'NONE',  ( -87.50000000000004263, 196.6227766016838245, -21.54065922853802562 ) ) ;
#6927 = LINE ( 'NONE', #5611, #1872 ) ;
#6928 = AXIS2_PLACEMENT_3D ( 'NONE', #8934, #899, #10188 ) ;
#6929 = CARTESIAN_POINT ( 'NONE',  ( -16.28901493728125160, 32.76428253546148284, -5.573780508339472028 ) ) ;
#6930 = TOROIDAL_SURFACE ( 'NONE', #985, 23.57392898041431195, 2.000000000000000000 ) ;
#6931 = ORIENTED_EDGE ( 'NONE', *, *, #16757, .F. ) ;
#6932 = ORIENTED_EDGE ( 'NONE', *, *, #6556, .F. ) ;
#6933 = VECTOR ( 'NONE', #2878, 1000.000000000000114 ) ;
#6934 = CARTESIAN_POINT ( 'NONE',  ( -72.50000000000000000, 197.1883573205068103, -20.88424858573643661 ) ) ;
#6935 = CARTESIAN_POINT ( 'NONE',  ( 16.61152767523946139, 141.2200844281568379, 17.35152312112458972 ) ) ;
#6936 = EDGE_CURVE ( 'NONE', #8817, #9579, #694, .T. ) ;
#6937 = ORIENTED_EDGE ( 'NONE', *, *, #5722, .T. ) ;
#6938 = APPLICATION_PROTOCOL_DEFINITION ( 'draft international standard', 'automotive_design', 1998, #8225 ) ;
#6939 = DIRECTION ( 'NONE',  ( 0.000000000000000000, 0.000000000000000000, -1.000000000000000000 ) ) ;
#6940 = DIRECTION ( 'NONE',  ( 1.000000000000000000, 0.000000000000000000, 0.000000000000000000 ) ) ;
#6941 = VECTOR ( 'NONE', #8982, 1000.000000000000000 ) ;
#6942 = CARTESIAN_POINT ( 'NONE',  ( 22.51550247401197069, 29.85017970947654575, -7.570302168957804057 ) ) ;
#6943 = CIRCLE ( 'NONE', #10058, 248.0000000000000000 ) ;
#6944 = CARTESIAN_POINT ( 'NONE',  ( 27.99999999999998224, 9.999999999999998224, 0.000000000000000000 ) ) ;
#6945 = FACE_OUTER_BOUND ( 'NONE', #12922, .T. ) ;
#6946 = AXIS2_PLACEMENT_3D ( 'NONE', #12469, #5738, #11125 ) ;
#6947 = VECTOR ( 'NONE', #648, 1000.000000000000000 ) ;
#6948 = VERTEX_POINT ( 'NONE', #17519 ) ;
#6949 = CARTESIAN_POINT ( 'NONE',  ( 24.93507336697353693, 29.86842105263157876, 0.000000000000000000 ) ) ;
#6950 = CIRCLE ( 'NONE', #15697, 33.00000000000000000 ) ;
#6951 = CARTESIAN_POINT ( 'NONE',  ( 27.99999999999998224, 9.999999999999998224, 28.00000000000001066 ) ) ;
#6952 = CARTESIAN_POINT ( 'NONE',  ( 34.99999999999999289, -20.00000000000000000, 39.99999999999998579 ) ) ;
#6953 = ADVANCED_FACE ( 'NONE', ( #10782 ), #5790, .T. ) ;
#6954 = CARTESIAN_POINT ( 'NONE',  ( -100.0000000000000000, 134.2062027339443944, 25.00000000000000000 ) ) ;
#6955 = DIRECTION ( 'NONE',  ( -1.000000000000000000, 0.000000000000000000, 0.000000000000000000 ) ) ;
#6956 = PRODUCT_DEFINITION_CONTEXT ( 'detailed design', #9124, 'design' ) ;
#6957 = ORIENTED_EDGE ( 'NONE', *, *, #4029, .T. ) ;
#6958 = CIRCLE ( 'NONE', #4967, 9.999999999999998224 ) ;
#6959 = EDGE_CURVE ( 'NONE', #7137, #16562, #12554, .T. ) ;
#6960 = LINE ( 'NONE', #234, #1433 ) ;
#6961 = CIRCLE ( 'NONE', #7795, 7.500000000000020428 ) ;
#6962 = ORIENTED_EDGE ( 'NONE', *, *, #4252, .T. ) ;
#6963 = EDGE_CURVE ( 'NONE', #2336, #9238, #2012, .T. ) ;
#6964 = CARTESIAN_POINT ( 'NONE',  ( -103.0000000000000142, 171.6227766016838245, -27.69059892324149530 ) ) ;
#6965 = EDGE_CURVE ( 'NONE', #9959, #11342, #13869, .T. ) ;
#6966 = ORIENTED_EDGE ( 'NONE', *, *, #8341, .F. ) ;
#6967 = CARTESIAN_POINT ( 'NONE',  ( -153.0000000000000284, 171.6227766016838245, 0.000000000000000000 ) ) ;
#6968 = FACE_OUTER_BOUND ( 'NONE', #3816, .T. ) ;
#6969 = AXIS2_PLACEMENT_3D ( 'NONE', #13565, #13646, #4267 ) ;
#6970 = VECTOR ( 'NONE', #4796, 1000.000000000000000 ) ;
#6971 = ORIENTED_EDGE ( 'NONE', *, *, #17461, .T. ) ;
#6972 = CARTESIAN_POINT ( 'NONE',  ( 22.50000000000000000, 196.6227766016838245, -21.54065922853802562 ) ) ;
#6973 = CARTESIAN_POINT ( 'NONE',  ( -50.00000000000000000, 154.3022685259950038, -9.999999999999900524 ) ) ;
#6974 = EDGE_CURVE ( 'NONE', #16869, #9238, #9773, .T. ) ;
#6975 = DIRECTION ( 'NONE',  ( -8.673617379884036705E-17, -8.673617379884037444E-16, 1.000000000000000000 ) ) ;
#6976 =( LENGTH_UNIT ( ) NAMED_UNIT ( * ) SI_UNIT ( .MILLI., .METRE. ) );
#6977 = CONICAL_SURFACE ( 'NONE', #9804, 2.499999999999998668, 1.029744260000002187 ) ;
#6978 = CARTESIAN_POINT ( 'NONE',  ( 26.46962346220079709, 137.6228726052619606, -8.310907492956932430 ) ) ;
#6979 = ORIENTED_EDGE ( 'NONE', *, *, #4719, .F. ) ;
#6980 = FACE_BOUND ( 'NONE', #9920, .T. ) ;
#6981 = CARTESIAN_POINT ( 'NONE',  ( -725.0000000000000000, 19.99999999999995737, -13.00000000000000000 ) ) ;
#6982 = ORIENTED_EDGE ( 'NONE', *, *, #15307, .T. ) ;
#6983 =( NAMED_UNIT ( * ) SI_UNIT ( $, .STERADIAN. ) SOLID_ANGLE_UNIT ( ) );
#6984 = AXIS2_PLACEMENT_3D ( 'NONE', #5321, #12042, #7390 ) ;
#6985 = CARTESIAN_POINT ( 'NONE',  ( -80.90398788703467403, 190.6868548533384171, -29.35237411376977334 ) ) ;
#6986 = CONICAL_SURFACE ( 'NONE', #7825, 2.499999999999998668, 1.029744260000002187 ) ;
#6987 = LINE ( 'NONE', #3181, #5600 ) ;
#6988 = CARTESIAN_POINT ( 'NONE',  ( -725.0000000000001137, 129.9999999999995453, -4.999999999999999112 ) ) ;
#6989 = DIRECTION ( 'NONE',  ( 0.000000000000000000, 0.000000000000000000, 1.000000000000000000 ) ) ;
#6990 = FACE_OUTER_BOUND ( 'NONE', #17295, .T. ) ;
#6991 = LINE ( 'NONE', #12297, #5636 ) ;
#6992 = EDGE_CURVE ( 'NONE', #8731, #6587, #15176, .T. ) ;
#6993 = EDGE_CURVE ( 'NONE', #8416, #16060, #8704, .T. ) ;
#6994 = DIRECTION ( 'NONE',  ( 1.000000000000000000, 0.000000000000000000, -0.000000000000000000 ) ) ;
#6995 = ADVANCED_FACE ( 'NONE', ( #16604 ), #15269, .F. ) ;
#6996 = AXIS2_PLACEMENT_3D ( 'NONE', #2823, #13629, #13900 ) ;
#6997 = FILL_AREA_STYLE ('',( #16395 ) ) ;
#6998 = VERTEX_POINT ( 'NONE', #14125 ) ;
#6999 = CARTESIAN_POINT ( 'NONE',  ( -15.53366225407947354, 31.76144936975385136, -11.66511309525283835 ) ) ;
#7000 = CIRCLE ( 'NONE', #13797, 8.000000000000000000 ) ;
#7001 = ORIENTED_EDGE ( 'NONE', *, *, #13635, .F. ) ;
#7002 = AXIS2_PLACEMENT_3D ( 'NONE', #9632, #258, #13543 ) ;
#7003 = CARTESIAN_POINT ( 'NONE',  ( 25.06493225369642630, 19.99999999999999645, -5.669446505520304491 ) ) ;
#7004 = AXIS2_PLACEMENT_3D ( 'NONE', #14053, #7310, #5803 ) ;
#7005 = CARTESIAN_POINT ( 'NONE',  ( 49.99999999999998579, 179.6227766016838245, 12.50000337241049309 ) ) ;
#7006 = ORIENTED_EDGE ( 'NONE', *, *, #14421, .T. ) ;
#7007 = CARTESIAN_POINT ( 'NONE',  ( -27.30244652380281778, 19.99999999999999645, 10.27378278477019080 ) ) ;
#7008 = CARTESIAN_POINT ( 'NONE',  ( 27.48361012698968864, 138.6227766016838245, -1.063447695028166570E-14 ) ) ;
#7009 = ORIENTED_EDGE ( 'NONE', *, *, #11335, .F. ) ;
#7010 = CARTESIAN_POINT ( 'NONE',  ( 26.21324911630662058, 153.1023373578139513, -27.31345131271288906 ) ) ;
#7011 = CARTESIAN_POINT ( 'NONE',  ( 1.559999999999998943, 1.732050807568885631, 0.000000000000000000 ) ) ;
#7012 = AXIS2_PLACEMENT_3D ( 'NONE', #14377, #11540, #6308 ) ;
#7013 = CIRCLE ( 'NONE', #4756, 20.00000000000000355 ) ;
#7014 = DIRECTION ( 'NONE',  ( -1.000000000000000000, 0.000000000000000000, 0.000000000000000000 ) ) ;
#7015 = CARTESIAN_POINT ( 'NONE',  ( 37.44048204095823706, 195.6584727333608669, -22.61345334826514275 ) ) ;
#7016 = DIRECTION ( 'NONE',  ( -1.000000000000000000, -6.938893903907228378E-16, -0.000000000000000000 ) ) ;
#7017 = ADVANCED_FACE ( 'NONE', ( #6055 ), #8871, .F. ) ;
#7018 = DIRECTION ( 'NONE',  ( -0.000000000000000000, -0.000000000000000000, 1.000000000000000000 ) ) ;
#7019 = CARTESIAN_POINT ( 'NONE',  ( -43.00000000000000000, 134.2062027339443944, -25.00000000000000000 ) ) ;
#7020 = EDGE_LOOP ( 'NONE', ( #15492, #13757 ) ) ;
#7021 = CARTESIAN_POINT ( 'NONE',  ( 14.58358448378887928, 141.6717822189192191, -18.11319387340528309 ) ) ;
#7022 = ORIENTED_EDGE ( 'NONE', *, *, #1955, .F. ) ;
#7023 = CYLINDRICAL_SURFACE ( 'NONE', #8746, 2.500000000000000444 ) ;
#7024 = CARTESIAN_POINT ( 'NONE',  ( -40.00000000000000000, 20.00000000000000000, -30.00000000000000355 ) ) ;
#7025 = CARTESIAN_POINT ( 'NONE',  ( -11.59473107857741425, 31.35552539902487723, -12.08231249604354574 ) ) ;
#7026 = VECTOR ( 'NONE', #3554, 1000.000000000000000 ) ;
#7027 = EDGE_LOOP ( 'NONE', ( #15745, #16522, #9145, #10788, #11004, #1265 ) ) ;
#7028 = ORIENTED_EDGE ( 'NONE', *, *, #11898, .F. ) ;
#7029 = LINE ( 'NONE', #1298, #14262 ) ;
#7030 = AXIS2_PLACEMENT_3D ( 'NONE', #8289, #8473, #68 ) ;
#7031 = CARTESIAN_POINT ( 'NONE',  ( -27.99999999999998224, 10.00000000000000000, 28.00000000000000355 ) ) ;
#7032 = CARTESIAN_POINT ( 'NONE',  ( 12.52734837489390785, 131.0783166553242722, 13.12014565386486176 ) ) ;
#7033 = EDGE_LOOP ( 'NONE', ( #7670, #43, #15861, #702 ) ) ;
#7034 = APPLICATION_PROTOCOL_DEFINITION ( 'draft international standard', 'automotive_design', 1998, #14001 ) ;
#7035 = DIRECTION ( 'NONE',  ( 0.000000000000000000, 0.000000000000000000, -1.000000000000000000 ) ) ;
#7036 = EDGE_CURVE ( 'NONE', #16418, #10459, #12868, .T. ) ;
#7037 = CARTESIAN_POINT ( 'NONE',  ( 0.000000000000000000, 20.00000000000000000, 0.000000000000000000 ) ) ;
#7038 = DIRECTION ( 'NONE',  ( 0.000000000000000000, 0.000000000000000000, -1.000000000000000000 ) ) ;
#7039 = VECTOR ( 'NONE', #9818, 1000.000000000000000 ) ;
#7040 = CARTESIAN_POINT ( 'NONE',  ( 39.99999999999998579, 4.000000000000007105, 30.00000000000001421 ) ) ;
#7041 = CARTESIAN_POINT ( 'NONE',  ( 17.53546816055560953, 18.00000000000000000, 24.87355917367171187 ) ) ;
#7042 = CIRCLE ( 'NONE', #3940, 11.93698985866628526 ) ;
#7043 = AXIS2_PLACEMENT_3D ( 'NONE', #8868, #6141, #8617 ) ;
#7044 = VERTEX_POINT ( 'NONE', #10120 ) ;
#7045 = CARTESIAN_POINT ( 'NONE',  ( 40.00000000000000711, 196.6227766016838245, 0.000000000000000000 ) ) ;
#7046 = DIRECTION ( 'NONE',  ( 1.000000000000000000, 0.000000000000000000, 0.000000000000000000 ) ) ;
#7047 = CYLINDRICAL_SURFACE ( 'NONE', #13684, 2.499999999999998668 ) ;
#7048 = CARTESIAN_POINT ( 'NONE',  ( -40.00000000000000000, 4.000000000000007105, 30.00000000000000711 ) ) ;
#7049 = CARTESIAN_POINT ( 'NONE',  ( -80.00000000000001421, 196.6227766016838245, -16.00000000000000000 ) ) ;
#7050 = ORIENTED_EDGE ( 'NONE', *, *, #6527, .T. ) ;
#7051 = ORIENTED_EDGE ( 'NONE', *, *, #10810, .T. ) ;
#7052 = AXIS2_PLACEMENT_3D ( 'NONE', #2983, #9708, #4148 ) ;
#7053 = CARTESIAN_POINT ( 'NONE',  ( 8.431728255697246155, 133.2562109147605156, 12.71722808757355949 ) ) ;
#7054 = CIRCLE ( 'NONE', #16949, 39.99999999999997868 ) ;
#7055 = ORIENTED_EDGE ( 'NONE', *, *, #11643, .F. ) ;
#7056 = VERTEX_POINT ( 'NONE', #8620 ) ;
#7057 = CARTESIAN_POINT ( 'NONE',  ( 48.00000000000000711, 163.6227766016838530, -12.50000337241049309 ) ) ;
#7058 = ADVANCED_FACE ( 'NONE', ( #16779, #10211 ), #3144, .T. ) ;
#7059 = CYLINDRICAL_SURFACE ( 'NONE', #14016, 20.00000000000000355 ) ;
#7060 = CARTESIAN_POINT ( 'NONE',  ( 17.00000000000000000, 154.3022685259950038, 9.999999999999900524 ) ) ;
#7061 = DIRECTION ( 'NONE',  ( 0.000000000000000000, 0.000000000000000000, -1.000000000000000000 ) ) ;
#7062 = ORIENTED_EDGE ( 'NONE', *, *, #12095, .F. ) ;
#7063 = CARTESIAN_POINT ( 'NONE',  ( 6.134011831684049731, 144.1839557653416080, 18.33333333333335702 ) ) ;
#7064 = AXIS2_PLACEMENT_3D ( 'NONE', #12044, #8233, #9640 ) ;
#7065 = PRODUCT_DEFINITION ( 'UNKNOWN', '', #16052, #5303 ) ;
#7066 = DIRECTION ( 'NONE',  ( 0.000000000000000000, 0.000000000000000000, 1.000000000000000000 ) ) ;
#7067 = DIRECTION ( 'NONE',  ( 1.000000000000000000, 0.000000000000000000, 0.000000000000000000 ) ) ;
#7068 = EDGE_CURVE ( 'NONE', #11112, #15769, #4372, .T. ) ;
#7069 = CIRCLE ( 'NONE', #7357, 20.00000000000000355 ) ;
#7070 = DIRECTION ( 'NONE',  ( -1.000000000000000000, -0.000000000000000000, 0.000000000000000000 ) ) ;
#7071 = EDGE_CURVE ( 'NONE', #1654, #4434, #12960, .T. ) ;
#7072 = CARTESIAN_POINT ( 'NONE',  ( 27.44407568426053246, 136.8394969516870958, -3.888888888888893725 ) ) ;
#7073 = ORIENTED_EDGE ( 'NONE', *, *, #9529, .F. ) ;
#7074 = FACE_BOUND ( 'NONE', #3205, .T. ) ;
#7075 = CARTESIAN_POINT ( 'NONE',  ( 26.85584576128377066, 139.3465472469502231, -6.878002324459898453 ) ) ;
#7076 = AXIS2_PLACEMENT_3D ( 'NONE', #12905, #9805, #16637 ) ;
#7077 = VECTOR ( 'NONE', #7836, 1000.000000000000000 ) ;
#7078 = VERTEX_POINT ( 'NONE', #6144 ) ;
#7079 = CARTESIAN_POINT ( 'NONE',  ( -82.99938094214050466, 191.4078883217828491, -28.87216486436161844 ) ) ;
#7080 = VECTOR ( 'NONE', #9616, 1000.000000000000000 ) ;
#7081 = DIRECTION ( 'NONE',  ( 0.000000000000000000, 0.000000000000000000, 1.000000000000000000 ) ) ;
#7082 = CARTESIAN_POINT ( 'NONE',  ( -91.33974596215564645, 171.6227766016838245, 0.000000000000000000 ) ) ;
#7083 = CARTESIAN_POINT ( 'NONE',  ( 27.48361012698968864, 138.6227766016838245, -1.063447695028166570E-14 ) ) ;
#7084 = DIRECTION ( 'NONE',  ( -1.000000000000000000, -0.000000000000000000, -0.000000000000000000 ) ) ;
#7085 = CARTESIAN_POINT ( 'NONE',  ( -39.68629150101524061, 122.0000000000000000, 9.686291501015231731 ) ) ;
#7086 = CARTESIAN_POINT ( 'NONE',  ( -80.94808030731641679, 201.5373699728806400, 13.93281245758934084 ) ) ;
#7087 = ORIENTED_EDGE ( 'NONE', *, *, #8673, .T. ) ;
#7088 = EDGE_LOOP ( 'NONE', ( #3058, #10316 ) ) ;
#7089 = CYLINDRICAL_SURFACE ( 'NONE', #7226, 10.00000000000000178 ) ;
#7090 = AXIS2_PLACEMENT_3D ( 'NONE', #2700, #14821, #12179 ) ;
#7091 = DIRECTION ( 'NONE',  ( -1.000000000000000000, 0.000000000000000000, 0.000000000000000000 ) ) ;
#7092 = ORIENTED_EDGE ( 'NONE', *, *, #1485, .T. ) ;
#7093 = DIRECTION ( 'NONE',  ( 1.000000000000000000, -0.000000000000000000, -0.000000000000000000 ) ) ;
#7094 = CARTESIAN_POINT ( 'NONE',  ( 49.99999999999998579, 163.6227766016838530, -15.00000337241049486 ) ) ;
#7095 = ORIENTED_EDGE ( 'NONE', *, *, #8979, .T. ) ;
#7096 = APPLICATION_CONTEXT ( 'automotive_design' ) ;
#7097 = EDGE_CURVE ( 'NONE', #13399, #8346, #7296, .T. ) ;
#7098 = CARTESIAN_POINT ( 'NONE',  ( 37.43684327452984206, 197.7246901893026632, -20.20962120078073809 ) ) ;
#7099 = CARTESIAN_POINT ( 'NONE',  ( -21.35874126517689220, 18.00000000000000355, 19.71585776365615317 ) ) ;
#7100 = DIRECTION ( 'NONE',  ( 1.000000000000000000, 0.000000000000000000, 0.000000000000000000 ) ) ;
#7101 = CARTESIAN_POINT ( 'NONE',  ( -207.6775903968322154, 175.2446381608502008, 3.971903508328557653 ) ) ;
#7102 = DIRECTION ( 'NONE',  ( -1.156482317317868274E-16, 1.000000000000000000, 0.000000000000000000 ) ) ;
#7103 = CARTESIAN_POINT ( 'NONE',  ( -90.80384757729339640, 204.6227766016838245, 0.000000000000000000 ) ) ;
#7104 = DIRECTION ( 'NONE',  ( 0.000000000000000000, 0.000000000000000000, 1.000000000000000000 ) ) ;
#7105 = ORIENTED_EDGE ( 'NONE', *, *, #1329, .T. ) ;
#7106 = DIRECTION ( 'NONE',  ( 0.000000000000000000, 0.000000000000000000, -1.000000000000000000 ) ) ;
#7107 = VERTEX_POINT ( 'NONE', #579 ) ;
#7108 = CARTESIAN_POINT ( 'NONE',  ( 27.44407568426044364, 136.8394969516870958, 3.888888888888887063 ) ) ;
#7109 = CIRCLE ( 'NONE', #608, 12.00000000000001421 ) ;
#7110 = CARTESIAN_POINT ( 'NONE',  ( -12.31336727611479631, 31.57746213708666971, -11.68681022658133806 ) ) ;
#7111 = ORIENTED_EDGE ( 'NONE', *, *, #6843, .F. ) ;
#7112 = EDGE_LOOP ( 'NONE', ( #1017, #1463 ) ) ;
#7113 = CARTESIAN_POINT ( 'NONE',  ( -187.6513770290094669, 171.1853623553243722, -0.7576236986489900405 ) ) ;
#7114 = ADVANCED_FACE ( 'NONE', ( #11369 ), #3319, .T. ) ;
#7115 = EDGE_CURVE ( 'NONE', #14296, #14117, #15099, .T. ) ;
#7116 = CARTESIAN_POINT ( 'NONE',  ( 6.134011831684049731, 134.2062027339443944, 13.00000000000000000 ) ) ;
#7117 = EDGE_CURVE ( 'NONE', #16986, #15774, #6229, .T. ) ;
#7118 = CARTESIAN_POINT ( 'NONE',  ( 18.85693063296981009, 140.6075696125688239, 16.22282984566914621 ) ) ;
#7119 = EDGE_CURVE ( 'NONE', #713, #3129, #11994, .T. ) ;
#7120 = ORIENTED_EDGE ( 'NONE', *, *, #1919, .T. ) ;
#7121 = CONTEXT_DEPENDENT_SHAPE_REPRESENTATION ( #11045, #10956 ) ;
#7122 = DIRECTION ( 'NONE',  ( 0.000000000000000000, 1.000000000000000000, -8.673617379884037444E-16 ) ) ;
#7123 = FACE_OUTER_BOUND ( 'NONE', #11669, .T. ) ;
#7124 = CARTESIAN_POINT ( 'NONE',  ( 15.56337975240373872, 125.2134999403456135, 4.999999999999997335 ) ) ;
#7125 = CARTESIAN_POINT ( 'NONE',  ( 196.0000000000000000, 159.6227766016838814, 5.571800142134975431 ) ) ;
#7126 = CARTESIAN_POINT ( 'NONE',  ( -27.98221281347037959, 20.00000000000000000, 4.999999999999999112 ) ) ;
#7127 = VERTEX_POINT ( 'NONE', #15528 ) ;
#7128 = CARTESIAN_POINT ( 'NONE',  ( -74.50191221171618849, 199.0501964078081016, -21.74862058155255795 ) ) ;
#7129 = CARTESIAN_POINT ( 'NONE',  ( -725.0000000000000000, 19.99999999999995737, -15.00000000000000000 ) ) ;
#7130 = CARTESIAN_POINT ( 'NONE',  ( 24.94691999498327206, 20.00000000000000355, -22.32501294936691139 ) ) ;
#7131 = DIRECTION ( 'NONE',  ( -1.000000000000000000, 0.000000000000000000, 0.000000000000000000 ) ) ;
#7132 = CARTESIAN_POINT ( 'NONE',  ( 225.0000000000000000, 89.99999999999997158, 4.999999999999999112 ) ) ;
#7133 = ORIENTED_EDGE ( 'NONE', *, *, #9213, .F. ) ;
#7134 = EDGE_CURVE ( 'NONE', #10459, #10626, #11983, .T. ) ;
#7135 = ORIENTED_EDGE ( 'NONE', *, *, #4257, .T. ) ;
#7136 = CARTESIAN_POINT ( 'NONE',  ( 8.856485326996372365, 132.9846638168478137, 12.59946789408625456 ) ) ;
#7137 = VERTEX_POINT ( 'NONE', #8717 ) ;
#7138 = CARTESIAN_POINT ( 'NONE',  ( -206.3689767832464668, 166.7044760491588988, 0.5444864983987496299 ) ) ;
#7139 = ORIENTED_EDGE ( 'NONE', *, *, #11898, .T. ) ;
#7140 =( LENGTH_UNIT ( ) NAMED_UNIT ( * ) SI_UNIT ( .MILLI., .METRE. ) );
#7141 = CARTESIAN_POINT ( 'NONE',  ( 22.94847233519770668, 144.0220640066157785, -18.10843944793623805 ) ) ;
#7142 = CARTESIAN_POINT ( 'NONE',  ( -33.00000000000000711, 171.6227766016838245, 0.000000000000000000 ) ) ;
#7143 = CARTESIAN_POINT ( 'NONE',  ( -32.64269715136552463, 118.7804878048780779, 4.500000000000000000 ) ) ;
#7144 = CARTESIAN_POINT ( 'NONE',  ( 30.00000000000000355, 196.6227766016838245, -35.00200000000000244 ) ) ;
#7145 = CARTESIAN_POINT ( 'NONE',  ( 22.56235622051156042, 18.00000000000227018, -7.873592366086867855 ) ) ;
#7146 = ORIENTED_EDGE ( 'NONE', *, *, #6432, .F. ) ;
#7147 = CARTESIAN_POINT ( 'NONE',  ( 25.11117529286356742, 145.4280468792802026, 20.09168135694114099 ) ) ;
#7148 = CARTESIAN_POINT ( 'NONE',  ( -100.0000000000000000, 100.0000000000000142, -6.000000000000000000 ) ) ;
#7149 = DIRECTION ( 'NONE',  ( 0.000000000000000000, 0.000000000000000000, -1.000000000000000000 ) ) ;
#7150 = DIRECTION ( 'NONE',  ( -0.000000000000000000, -1.000000000000000000, -0.000000000000000000 ) ) ;
#7151 = EDGE_CURVE ( 'NONE', #9019, #4348, #14208, .T. ) ;
#7152 = PRODUCT_DEFINITION_SHAPE ( 'NONE', 'NONE',  #7065 ) ;
#7153 = ADVANCED_FACE ( 'NONE', ( #4822 ), #4523, .T. ) ;
#7154 = CARTESIAN_POINT ( 'NONE',  ( -7.379000772445021283, 18.00000000000000000, -25.00000000000000355 ) ) ;
#7155 = ORIENTED_EDGE ( 'NONE', *, *, #4525, .T. ) ;
#7156 = DIRECTION ( 'NONE',  ( -1.000000000000000000, 0.000000000000000000, 0.000000000000000000 ) ) ;
#7157 = ORIENTED_EDGE ( 'NONE', *, *, #9878, .F. ) ;
#7158 = SURFACE_STYLE_USAGE ( .BOTH. , #16468 ) ;
#7159 = CARTESIAN_POINT ( 'NONE',  ( -84.02588075151039959, 192.1541050315148595, -28.34722919022667043 ) ) ;
#7160 = EDGE_CURVE ( 'NONE', #9285, #3708, #14233, .T. ) ;
#7161 = DIRECTION ( 'NONE',  ( -1.000000000000000000, 0.000000000000000000, 0.000000000000000000 ) ) ;
#7162 = CARTESIAN_POINT ( 'NONE',  ( 26.58318862804039640, 192.9554221994867476, 25.17938093289615509 ) ) ;
#7163 = PLANE ( 'NONE',  #1039 ) ;
#7164 = FACE_OUTER_BOUND ( 'NONE', #4386, .T. ) ;
#7165 = DIRECTION ( 'NONE',  ( 1.000000000000000000, 0.000000000000000000, 0.000000000000000000 ) ) ;
#7166 = CARTESIAN_POINT ( 'NONE',  ( 6.134011831684049731, 144.1839557653416080, -18.33333333333335702 ) ) ;
#7167 = FACE_BOUND ( 'NONE', #11236, .T. ) ;
#7168 = EDGE_LOOP ( 'NONE', ( #2087, #14212, #11177, #4964 ) ) ;
#7169 = ORIENTED_EDGE ( 'NONE', *, *, #11708, .F. ) ;
#7170 = CARTESIAN_POINT ( 'NONE',  ( 24.60025152864608700, 29.87271304632927027, -7.586598161752979408 ) ) ;
#7171 = CARTESIAN_POINT ( 'NONE',  ( 27.44407568426044008, 138.8271129316868837, -3.666666666666658081 ) ) ;
#7172 = VERTEX_POINT ( 'NONE', #5433 ) ;
#7173 = DIRECTION ( 'NONE',  ( 0.000000000000000000, 0.8660254037844413721, -0.4999999999999952816 ) ) ;
#7174 = DIRECTION ( 'NONE',  ( 0.000000000000000000, 0.000000000000000000, 1.000000000000000000 ) ) ;
#7175 = VERTEX_POINT ( 'NONE', #1710 ) ;
#7176 = CARTESIAN_POINT ( 'NONE',  ( 32.27956779150308364, 153.7735974263994194, -27.75644086540373934 ) ) ;
#7177 = ADVANCED_FACE ( 'NONE', ( #2773 ), #8330, .T. ) ;
#7178 = CARTESIAN_POINT ( 'NONE',  ( -17.58288004918493996, 18.00000000000000000, 22.43027208364173575 ) ) ;
#7179 = DIRECTION ( 'NONE',  ( 0.000000000000000000, 0.000000000000000000, -1.000000000000000000 ) ) ;
#7180 = AXIS2_PLACEMENT_3D ( 'NONE', #7503, #12913, #7854 ) ;
#7181 = DIRECTION ( 'NONE',  ( -1.000000000000000000, 0.000000000000000000, 0.000000000000000000 ) ) ;
#7182 = FACE_OUTER_BOUND ( 'NONE', #17093, .T. ) ;
#7183 = DIRECTION ( 'NONE',  ( 0.000000000000000000, 0.000000000000000000, 1.000000000000000000 ) ) ;
#7184 = CARTESIAN_POINT ( 'NONE',  ( -74.72505082391214160, 141.2912748254776147, -13.00000000000000000 ) ) ;
#7185 = EDGE_LOOP ( 'NONE', ( #201, #14566, #1606, #11825 ) ) ;
#7186 = DIRECTION ( 'NONE',  ( 1.000000000000000000, 0.000000000000000000, 0.000000000000000000 ) ) ;
#7187 = ADVANCED_FACE ( 'NONE', ( #1618 ), #199, .T. ) ;
#7188 = ORIENTED_EDGE ( 'NONE', *, *, #5030, .F. ) ;
#7189 = FACE_OUTER_BOUND ( 'NONE', #16403, .T. ) ;
#7190 = LINE ( 'NONE', #4460, #4424 ) ;
#7191 = EDGE_LOOP ( 'NONE', ( #4445, #1009, #7621, #7416, #17238, #924 ) ) ;
#7192 = ORIENTED_EDGE ( 'NONE', *, *, #8349, .T. ) ;
#7193 = CARTESIAN_POINT ( 'NONE',  ( -23.00000000000001421, 122.0000000000000284, 4.999999999999999112 ) ) ;
#7194 = AXIS2_PLACEMENT_3D ( 'NONE', #12065, #15144, #3024 ) ;
#7195 = AXIS2_PLACEMENT_3D ( 'NONE', #15246, #8696, #3122 ) ;
#7196 = PLANE ( 'NONE',  #10730 ) ;
#7197 = CARTESIAN_POINT ( 'NONE',  ( 15.82262738632537946, 137.2266821760960340, 8.447647312139547893 ) ) ;
#7198 = ORIENTED_EDGE ( 'NONE', *, *, #5382, .F. ) ;
#7199 = CYLINDRICAL_SURFACE ( 'NONE', #10769, 6.000000000000005329 ) ;
#7200 = DIRECTION ( 'NONE',  ( 0.01578383822436034076, -0.1110972697184772484, -0.9936841888205766304 ) ) ;
#7201 = CARTESIAN_POINT ( 'NONE',  ( -75.46415429630739879, 194.4969340293140476, 23.78882387388087238 ) ) ;
#7202 = CARTESIAN_POINT ( 'NONE',  ( 14.93242934743711992, 30.00000000000000000, 15.00000000000000000 ) ) ;
#7203 = CARTESIAN_POINT ( 'NONE',  ( 21.98114852961722576, 18.00000000000000000, 23.72829316725777815 ) ) ;
#7204 = CARTESIAN_POINT ( 'NONE',  ( -45.00000000000000000, 140.0000000000000000, 0.000000000000000000 ) ) ;
#7205 = AXIS2_PLACEMENT_3D ( 'NONE', #10530, #14260, #9031 ) ;
#7206 = VERTEX_POINT ( 'NONE', #4103 ) ;
#7207 = DIRECTION ( 'NONE',  ( 0.000000000000000000, 1.000000000000000000, 0.000000000000000000 ) ) ;
#7208 = EDGE_CURVE ( 'NONE', #134, #12318, #2111, .T. ) ;
#7209 = EDGE_CURVE ( 'NONE', #903, #118, #6338, .T. ) ;
#7211 = DIRECTION ( 'NONE',  ( -0.000000000000000000, -0.000000000000000000, -1.000000000000000000 ) ) ;
#7210 = CIRCLE ( 'NONE', #10893, 2.500000000000002220 ) ;
#7212 = EDGE_CURVE ( 'NONE', #6066, #10900, #11140, .T. ) ;
#7213 = CARTESIAN_POINT ( 'NONE',  ( -15.00000000000002665, 130.0000000000000000, 15.00000000000000000 ) ) ;
#7214 = DIRECTION ( 'NONE',  ( 0.000000000000000000, 0.8660254037844413721, 0.4999999999999952816 ) ) ;
#7215 = CARTESIAN_POINT ( 'NONE',  ( 1.559999999999998943, 0.000000000000000000, 0.000000000000000000 ) ) ;
#7216 = ORIENTED_EDGE ( 'NONE', *, *, #9430, .T. ) ;
#7217 = ORIENTED_EDGE ( 'NONE', *, *, #11179, .F. ) ;
#7218 = ORIENTED_EDGE ( 'NONE', *, *, #15267, .T. ) ;
#7219 = CARTESIAN_POINT ( 'NONE',  ( -15.00000000000002132, 90.00000000000000000, -4.999999999999999112 ) ) ;
#7220 = VERTEX_POINT ( 'NONE', #8073 ) ;
#7221 = DIRECTION ( 'NONE',  ( -1.000000000000000000, -0.000000000000000000, -0.000000000000000000 ) ) ;
#7222 = CIRCLE ( 'NONE', #15420, 12.00000000000000000 ) ;
#7223 = ORIENTED_EDGE ( 'NONE', *, *, #12229, .F. ) ;
#7224 = DIRECTION ( 'NONE',  ( -0.000000000000000000, -0.000000000000000000, -1.000000000000000000 ) ) ;
#7225 = VECTOR ( 'NONE', #3251, 1000.000000000000114 ) ;
#7226 = AXIS2_PLACEMENT_3D ( 'NONE', #8502, #3009, #15045 ) ;
#7227 = CARTESIAN_POINT ( 'NONE',  ( 48.00000000000000711, 191.6227766016837677, 3.071800142134975431 ) ) ;
#7228 = AXIS2_PLACEMENT_3D ( 'NONE', #16086, #15812, #1021 ) ;
#7229 = CARTESIAN_POINT ( 'NONE',  ( -197.9999999999999716, 171.6227766016838245, 0.000000000000000000 ) ) ;
#7230 = CARTESIAN_POINT ( 'NONE',  ( -68.00000000000000000, 171.6227766016838245, 0.000000000000000000 ) ) ;
#7231 = ORIENTED_EDGE ( 'NONE', *, *, #17518, .F. ) ;
#7232 = CARTESIAN_POINT ( 'NONE',  ( 33.63865905896372510, 143.1809062453614843, 16.74061342279919984 ) ) ;
#7233 = CARTESIAN_POINT ( 'NONE',  ( -5.000000000000004441, 171.6227766016838245, 0.000000000000000000 ) ) ;
#7234 = CARTESIAN_POINT ( 'NONE',  ( -70.00000000000000000, 204.6227766016838245, 2.020667218593133100E-15 ) ) ;
#7235 = AXIS2_PLACEMENT_3D ( 'NONE', #9494, #9847, #1459 ) ;
#7236 = VECTOR ( 'NONE', #13865, 1000.000000000000000 ) ;
#7237 = VECTOR ( 'NONE', #14758, 1000.000000000000000 ) ;
#7238 = CARTESIAN_POINT ( 'NONE',  ( -23.00000000000000000, 122.0000000000000284, -15.00000000000000000 ) ) ;
#7239 = EDGE_LOOP ( 'NONE', ( #15223, #1691, #10121, #11615 ) ) ;
#7240 = CARTESIAN_POINT ( 'NONE',  ( -40.00000000000000000, 20.00000000000000000, 0.000000000000000000 ) ) ;
#7241 = VERTEX_POINT ( 'NONE', #10994 ) ;
#7242 = CARTESIAN_POINT ( 'NONE',  ( 0.000000000000000000, 18.00000000000000355, 0.000000000000000000 ) ) ;
#7244 = ORIENTED_EDGE ( 'NONE', *, *, #3322, .F. ) ;
#7243 = CIRCLE ( 'NONE', #1879, 30.00000000000000000 ) ;
#7245 = AXIS2_PLACEMENT_3D ( 'NONE', #2047, #7440, #12841 ) ;
#7246 = DIRECTION ( 'NONE',  ( 0.000000000000000000, 0.000000000000000000, -1.000000000000000000 ) ) ;
#7247 = VECTOR ( 'NONE', #8433, 1000.000000000000000 ) ;
#7248 = DIRECTION ( 'NONE',  ( -1.000000000000000000, -0.000000000000000000, -0.000000000000000000 ) ) ;
#7249 = EDGE_CURVE ( 'NONE', #4808, #12895, #6849, .T. ) ;
#7250 = DIRECTION ( 'NONE',  ( -1.000000000000000000, 0.000000000000000000, 0.000000000000000000 ) ) ;
#7251 = VERTEX_POINT ( 'NONE', #17475 ) ;
#7252 = DIRECTION ( 'NONE',  ( 0.000000000000000000, 0.000000000000000000, 1.000000000000000000 ) ) ;
#7253 = LINE ( 'NONE', #4606, #12405 ) ;
#7254 = CARTESIAN_POINT ( 'NONE',  ( -79.09267923946974577, 201.5450689758321232, 13.91624649103837719 ) ) ;
#7255 =( LENGTH_UNIT ( ) NAMED_UNIT ( * ) SI_UNIT ( .MILLI., .METRE. ) );
#7256 = ORIENTED_EDGE ( 'NONE', *, *, #6677, .T. ) ;
#7257 = ORIENTED_EDGE ( 'NONE', *, *, #2055, .T. ) ;
#7258 = CARTESIAN_POINT ( 'NONE',  ( 31.20232444246483894, 19.99999999999999645, -16.65183244246150451 ) ) ;
#7259 = AXIS2_PLACEMENT_3D ( 'NONE', #6559, #2582, #11949 ) ;
#7260 = DIRECTION ( 'NONE',  ( 1.000000000000000000, 0.000000000000000000, 0.000000000000000000 ) ) ;
#7261 = CIRCLE ( 'NONE', #7535, 8.000000000000000000 ) ;
#7262 = VERTEX_POINT ( 'NONE', #32 ) ;
#7263 =( GEOMETRIC_REPRESENTATION_CONTEXT ( 3 ) GLOBAL_UNCERTAINTY_ASSIGNED_CONTEXT ( ( #13687 ) ) GLOBAL_UNIT_ASSIGNED_CONTEXT ( ( #15973, #14476, #10388 ) ) REPRESENTATION_CONTEXT ( 'NONE', 'WORKASPACE' ) );
#7264 = DIRECTION ( 'NONE',  ( 0.000000000000000000, 0.000000000000000000, 1.000000000000000000 ) ) ;
#7265 = CARTESIAN_POINT ( 'NONE',  ( -27.98221281347037959, 30.00000000000000000, 15.00000000000000000 ) ) ;
#7266 = EDGE_LOOP ( 'NONE', ( #13404, #7192, #905, #7399, #11081 ) ) ;
#7267 = DIRECTION ( 'NONE',  ( 0.000000000000000000, -1.224646799147353207E-16, 1.000000000000000000 ) ) ;
#7268 = DIRECTION ( 'NONE',  ( -0.000000000000000000, -1.000000000000000000, -0.000000000000000000 ) ) ;
#7269 = ADVANCED_FACE ( 'NONE', ( #16324 ), #289, .T. ) ;
#7270 = DIRECTION ( 'NONE',  ( 0.000000000000000000, 0.000000000000000000, -1.000000000000000000 ) ) ;
#7271 = PLANE ( 'NONE',  #14004 ) ;
#7272 = DIRECTION ( 'NONE',  ( 0.000000000000000000, -1.000000000000000000, 0.000000000000000000 ) ) ;
#7273 = CIRCLE ( 'NONE', #13781, 8.000000000000007105 ) ;
#7274 = DIRECTION ( 'NONE',  ( -1.156482317317868274E-16, 1.000000000000000000, 0.000000000000000000 ) ) ;
#7275 = CARTESIAN_POINT ( 'NONE',  ( -72.79003115184357853, 144.4916047800714693, -18.80562413441370850 ) ) ;
#7276 = ORIENTED_EDGE ( 'NONE', *, *, #14691, .T. ) ;
#7277 = EDGE_CURVE ( 'NONE', #8476, #1481, #9445, .T. ) ;
#7278 = ORIENTED_EDGE ( 'NONE', *, *, #13141, .F. ) ;
#7279 = ADVANCED_FACE ( 'NONE', ( #5513, #4192 ), #5343, .F. ) ;
#7280 = DIRECTION ( 'NONE',  ( 0.000000000000000000, 0.5000000000000011102, -0.8660254037844379305 ) ) ;
#7281 = EDGE_CURVE ( 'NONE', #3225, #12025, #12010, .T. ) ;
#7282 = DIRECTION ( 'NONE',  ( 1.000000000000000000, 0.000000000000000000, 0.000000000000000000 ) ) ;
#7283 = ORIENTED_EDGE ( 'NONE', *, *, #5752, .F. ) ;
#7284 = LINE ( 'NONE', #4635, #9162 ) ;
#7285 = CARTESIAN_POINT ( 'NONE',  ( 27.44407568426047206, 136.8394969516870958, 3.888888888888889728 ) ) ;
#7286 = CARTESIAN_POINT ( 'NONE',  ( 25.02538947967125793, 138.3580044269788800, 10.92703196337285299 ) ) ;
#7287 = AXIS2_PLACEMENT_3D ( 'NONE', #5258, #7999, #17486 ) ;
#7288 = ORIENTED_EDGE ( 'NONE', *, *, #12863, .T. ) ;
#7289 = ITEM_DEFINED_TRANSFORMATION ( 'NONE', 'NONE', #14065,  #3583 ) ;
#7290 = CARTESIAN_POINT ( 'NONE',  ( 48.00000000000000711, 187.6227766016837961, 12.50000337241049309 ) ) ;
#7291 = FACE_OUTER_BOUND ( 'NONE', #4248, .T. ) ;
#7292 = CARTESIAN_POINT ( 'NONE',  ( 196.0000000000000000, 183.6227766016837961, -5.571800142134975431 ) ) ;
#7293 = CARTESIAN_POINT ( 'NONE',  ( -38.00000000000000000, 18.00000000000000355, 28.00000000000000355 ) ) ;
#7294 = CARTESIAN_POINT ( 'NONE',  ( 17.52334770333193248, 18.00000000000113332, 12.62810114740270606 ) ) ;
#7295 = PRODUCT_DEFINITION_SHAPE ( 'NONE', 'NONE',  #17537 ) ;
#7296 = LINE ( 'NONE', #12701, #10573 ) ;
#7297 = EDGE_LOOP ( 'NONE', ( #7157, #14624, #5675, #9515 ) ) ;
#7298 = CARTESIAN_POINT ( 'NONE',  ( -32.66708739526796279, 101.0000000000000142, 4.722170599040663497 ) ) ;
#7299 = AXIS2_PLACEMENT_3D ( 'NONE', #8806, #14210, #6146 ) ;
#7300 = PLANE ( 'NONE',  #26 ) ;
#7301 = ORIENTED_EDGE ( 'NONE', *, *, #4463, .T. ) ;
#7302 = DIRECTION ( 'NONE',  ( 0.000000000000000000, 0.000000000000000000, -1.000000000000000000 ) ) ;
#7303 = CIRCLE ( 'NONE', #14648, 40.99999999999997868 ) ;
#7304 = FACE_BOUND ( 'NONE', #5033, .T. ) ;
#7305 = EDGE_LOOP ( 'NONE', ( #11526, #1887, #1913, #6548 ) ) ;
#7306 = ORIENTED_EDGE ( 'NONE', *, *, #11443, .T. ) ;
#7307 = ORIENTED_EDGE ( 'NONE', *, *, #9201, .T. ) ;
#7308 = CARTESIAN_POINT ( 'NONE',  ( 10.76597736162413632, 139.9178931572356532, 11.43282512092270053 ) ) ;
#7309 = ORIENTED_EDGE ( 'NONE', *, *, #15450, .F. ) ;
#7310 = DIRECTION ( 'NONE',  ( -0.000000000000000000, -0.000000000000000000, -1.000000000000000000 ) ) ;
#7311 = ORIENTED_EDGE ( 'NONE', *, *, #2781, .F. ) ;
#7312 = ADVANCED_FACE ( 'NONE', ( #12323 ), #16416, .F. ) ;
#7313 = SURFACE_SIDE_STYLE ('',( #10139 ) ) ;
#7314 = EDGE_CURVE ( 'NONE', #15354, #5870, #5691, .T. ) ;
#7315 = AXIS2_PLACEMENT_3D ( 'NONE', #9301, #10808, #10722 ) ;
#7316 = DIRECTION ( 'NONE',  ( -0.000000000000000000, -0.000000000000000000, -1.000000000000000000 ) ) ;
#7317 = EDGE_CURVE ( 'NONE', #1461, #14379, #2960, .T. ) ;
#7318 = VECTOR ( 'NONE', #11925, 1000.000000000000114 ) ;
#7319 = CARTESIAN_POINT ( 'NONE',  ( 15.04007972439966956, 126.3543340278276190, 7.435061541642935978 ) ) ;
#7320 = CARTESIAN_POINT ( 'NONE',  ( -85.00000000000002842, 196.6227766016838245, -12.99999999999999822 ) ) ;
#7321 = LINE ( 'NONE', #15367, #15125 ) ;
#7322 = ORIENTED_EDGE ( 'NONE', *, *, #2498, .T. ) ;
#7323 = CARTESIAN_POINT ( 'NONE',  ( 25.00000000000001066, 146.0036328918050970, 20.82208359987472335 ) ) ;
#7324 = DIRECTION ( 'NONE',  ( -0.000000000000000000, -0.000000000000000000, -1.000000000000000000 ) ) ;
#7325 = CARTESIAN_POINT ( 'NONE',  ( -100.0000000000000000, 143.0439382767972347, -16.49999999999984368 ) ) ;
#7326 = CARTESIAN_POINT ( 'NONE',  ( -7.379000772444995526, 20.00000000000000000, -25.00000000000000000 ) ) ;
#7327 = CIRCLE ( 'NONE', #14121, 19.49999999999998224 ) ;
#7328 = APPLICATION_CONTEXT ( 'automotive_design' ) ;
#7329 = VECTOR ( 'NONE', #3054, 1000.000000000000000 ) ;
#7330 = AXIS2_PLACEMENT_3D ( 'NONE', #16511, #4380, #11098 ) ;
#7331 = CARTESIAN_POINT ( 'NONE',  ( -21.99999999999998579, 10.00000000000000000, -16.00000000000000000 ) ) ;
#7332 = EDGE_LOOP ( 'NONE', ( #10504, #8442, #2175, #3865, #15750, #12956, #12820, #1797 ) ) ;
#7333 = CARTESIAN_POINT ( 'NONE',  ( -80.00000000000002842, 146.6227766016838245, 0.000000000000000000 ) ) ;
#7334 = ORIENTED_EDGE ( 'NONE', *, *, #10599, .F. ) ;
#7335 = EDGE_CURVE ( 'NONE', #10429, #12327, #8425, .T. ) ;
#7336 = SHAPE_REPRESENTATION_RELATIONSHIP ( 'NONE' , 'NONE' ,  #17073, #2569 ) ;
#7337 = EDGE_CURVE ( 'NONE', #9311, #8718, #9840, .T. ) ;
#7338 = CARTESIAN_POINT ( 'NONE',  ( 24.48161681970857018, 138.6020828307752879, 11.64873334838780572 ) ) ;
#7339 = CYLINDRICAL_SURFACE ( 'NONE', #14942, 6.000000000000005329 ) ;
#7340 = VECTOR ( 'NONE', #1570, 1000.000000000000000 ) ;
#7341 = CIRCLE ( 'NONE', #4514, 14.16444493696511486 ) ;
#7342 = AXIS2_PLACEMENT_3D ( 'NONE', #13024, #10263, #4618 ) ;
#7343 = CARTESIAN_POINT ( 'NONE',  ( -18.25212770525997286, 32.30769230769230660, -4.999999999999999112 ) ) ;
#7344 = ORIENTED_EDGE ( 'NONE', *, *, #2529, .T. ) ;
#7345 = DIRECTION ( 'NONE',  ( 1.000000000000000000, 0.000000000000000000, -0.000000000000000000 ) ) ;
#7346 = CARTESIAN_POINT ( 'NONE',  ( 49.99999999999998579, 171.6227766016838245, -12.50000337241049131 ) ) ;
#7347 = CARTESIAN_POINT ( 'NONE',  ( -79.78392266530065058, 201.6195082837481323, 13.75486997215864093 ) ) ;
#7348 = LINE ( 'NONE', #1857, #11171 ) ;
#7349 = EDGE_LOOP ( 'NONE', ( #11455, #2568, #8921, #16429 ) ) ;
#7350 = ORIENTED_EDGE ( 'NONE', *, *, #7473, .F. ) ;
#7351 = DIRECTION ( 'NONE',  ( -1.000000000000000000, 0.000000000000000000, 0.000000000000000000 ) ) ;
#7352 = AXIS2_PLACEMENT_3D ( 'NONE', #9535, #6884, #5396 ) ;
#7353 = CARTESIAN_POINT ( 'NONE',  ( 17.57170338634705331, 142.7189882356449857, -15.92841986281182187 ) ) ;
#7354 = EDGE_LOOP ( 'NONE', ( #7998, #7396, #2720, #11242, #1725 ) ) ;
#7355 = EDGE_CURVE ( 'NONE', #668, #12793, #8598, .T. ) ;
#7356 = CARTESIAN_POINT ( 'NONE',  ( -70.00000000000000000, 171.6227766016838245, 0.000000000000000000 ) ) ;
#7357 = AXIS2_PLACEMENT_3D ( 'NONE', #14605, #17173, #7695 ) ;
#7358 = CARTESIAN_POINT ( 'NONE',  ( 6.134011831684059501, 144.1839557653415795, -18.33333333333333215 ) ) ;
#7359 = ORIENTED_EDGE ( 'NONE', *, *, #917, .T. ) ;
#7360 = CARTESIAN_POINT ( 'NONE',  ( 2.950000000000001066, 3.306546357697852747E-16, -2.699999999999999289 ) ) ;
#7361 = UNCERTAINTY_MEASURE_WITH_UNIT (LENGTH_MEASURE( 1.000000000000000082E-05 ), #7140, 'distance_accuracy_value', 'NONE');
#7362 =( BOUNDED_CURVE ( )  B_SPLINE_CURVE ( 3, ( #3551, #4960, #3643, #12939 ),
 .UNSPECIFIED., .F., .F. ) 
 B_SPLINE_CURVE_WITH_KNOTS ( ( 4, 4 ),
 ( 4.712388980384692339, 6.283185307179586232 ),
 .UNSPECIFIED. ) 
 CURVE ( )  GEOMETRIC_REPRESENTATION_ITEM ( )  RATIONAL_B_SPLINE_CURVE ( ( 1.000000000000000000, 0.8047378541243654926, 0.8047378541243654926, 1.000000000000000000 ) ) 
 REPRESENTATION_ITEM ( '' )  );
#7363 = CARTESIAN_POINT ( 'NONE',  ( -34.99999999999999289, 130.0000000000000000, -15.00000000000000000 ) ) ;
#7364 = PLANE ( 'NONE',  #2728 ) ;
#7365 = FACE_BOUND ( 'NONE', #15473, .T. ) ;
#7366 = VECTOR ( 'NONE', #16634, 1000.000000000000000 ) ;
#7367 = CARTESIAN_POINT ( 'NONE',  ( -27.30244652380281778, 18.00000000000000000, 10.27378278477019080 ) ) ;
#7368 = LINE ( 'NONE', #13926, #12284 ) ;
#7369 = AXIS2_PLACEMENT_3D ( 'NONE', #7478, #498, #10227 ) ;
#7370 = DIRECTION ( 'NONE',  ( -0.000000000000000000, -0.000000000000000000, 1.000000000000000000 ) ) ;
#7371 = EDGE_LOOP ( 'NONE', ( #2952, #442, #6421, #12195, #15616 ) ) ;
#7372 = FACE_BOUND ( 'NONE', #3259, .T. ) ;
#7373 = B_SPLINE_CURVE_WITH_KNOTS ( 'NONE', 3,
 ( #17403, #5273, #13607, #16085 ),
 .UNSPECIFIED., .F., .F.,
 ( 4, 4 ),
 ( 0.000000000000000000, 0.0004807729677303993116 ),
 .UNSPECIFIED. ) ;
#7374 = VERTEX_POINT ( 'NONE', #5770 ) ;
#7375 = DIRECTION ( 'NONE',  ( 1.000000000000000000, -0.000000000000000000, -0.000000000000000000 ) ) ;
#7376 = FACE_OUTER_BOUND ( 'NONE', #3756, .T. ) ;
#7377 = ORIENTED_EDGE ( 'NONE', *, *, #6808, .T. ) ;
#7378 = EDGE_CURVE ( 'NONE', #9236, #15970, #15413, .T. ) ;
#7379 = CARTESIAN_POINT ( 'NONE',  ( 34.93420767853314146, 20.00000000000000000, 6.320602137672510779 ) ) ;
#7380 = VECTOR ( 'NONE', #4569, 1000.000000000000000 ) ;
#7381 = CARTESIAN_POINT ( 'NONE',  ( 25.49876332522151401, 19.99999999999999645, 21.99427390110736624 ) ) ;
#7382 = DIRECTION ( 'NONE',  ( 0.000000000000000000, 0.000000000000000000, -1.000000000000000000 ) ) ;
#7383 = EDGE_LOOP ( 'NONE', ( #9937, #12708 ) ) ;
#7384 = DIRECTION ( 'NONE',  ( 2.312964634635742464E-16, 0.000000000000000000, 1.000000000000000000 ) ) ;
#7385 = EDGE_CURVE ( 'NONE', #4882, #13912, #7443, .T. ) ;
#7386 = DIRECTION ( 'NONE',  ( -0.000000000000000000, -0.000000000000000000, -1.000000000000000000 ) ) ;
#7387 = EDGE_CURVE ( 'NONE', #16546, #713, #4543, .T. ) ;
#7388 = CARTESIAN_POINT ( 'NONE',  ( -80.18730344621531003, 191.6224348813836116, 26.24906986711107848 ) ) ;
#7389 = DIRECTION ( 'NONE',  ( -1.000000000000000000, 0.000000000000000000, 0.000000000000000000 ) ) ;
#7390 = DIRECTION ( 'NONE',  ( 0.000000000000000000, 0.000000000000000000, -1.000000000000000000 ) ) ;
#7391 = DIRECTION ( 'NONE',  ( 0.000000000000000000, 0.000000000000000000, 1.000000000000000000 ) ) ;
#7392 = ORIENTED_EDGE ( 'NONE', *, *, #12412, .F. ) ;
#7393 = CARTESIAN_POINT ( 'NONE',  ( -208.1430079281944074, 169.2505655449146786, -4.108790076600865149 ) ) ;
#7394 = CIRCLE ( 'NONE', #8510, 5.000000000000004441 ) ;
#7395 = CARTESIAN_POINT ( 'NONE',  ( -22.79696676584442017, 19.99999999999999645, -18.34105320469109301 ) ) ;
#7396 = ORIENTED_EDGE ( 'NONE', *, *, #16739, .T. ) ;
#7397 = DIRECTION ( 'NONE',  ( -0.000000000000000000, -0.000000000000000000, -1.000000000000000000 ) ) ;
#7398 = FACE_BOUND ( 'NONE', #11710, .T. ) ;
#7399 = ORIENTED_EDGE ( 'NONE', *, *, #8887, .F. ) ;
#7400 = ORIENTED_EDGE ( 'NONE', *, *, #1865, .T. ) ;
#7401 = ORIENTED_EDGE ( 'NONE', *, *, #8795, .F. ) ;
#7402 = ORIENTED_EDGE ( 'NONE', *, *, #16890, .T. ) ;
#7403 = PLANE ( 'NONE',  #7934 ) ;
#7404 = CARTESIAN_POINT ( 'NONE',  ( 13.21952030233119046, 128.8713892059273860, 10.07325499884888664 ) ) ;
#7405 = EDGE_CURVE ( 'NONE', #5635, #8295, #9583, .T. ) ;
#7406 = FACE_OUTER_BOUND ( 'NONE', #11127, .T. ) ;
#7407 = CARTESIAN_POINT ( 'NONE',  ( 6.134011831684049731, 134.2062027339443944, -13.00000000000000000 ) ) ;
#7408 = VERTEX_POINT ( 'NONE', #726 ) ;
#7409 = CYLINDRICAL_SURFACE ( 'NONE', #15195, 2.499999999999999112 ) ;
#7410 = DIRECTION ( 'NONE',  ( 2.312964634635742464E-16, 0.000000000000000000, 1.000000000000000000 ) ) ;
#7411 = CARTESIAN_POINT ( 'NONE',  ( -25.00000000000002132, 120.0000000000000284, -5.000000000000023093 ) ) ;
#7412 = CARTESIAN_POINT ( 'NONE',  ( -7.379000772444995526, 20.00000000000000355, -15.00000000000000178 ) ) ;
#7413 = CARTESIAN_POINT ( 'NONE',  ( 49.99999999999998579, 175.6227766016838245, 3.071800142134975431 ) ) ;
#7414 = EDGE_CURVE ( 'NONE', #3416, #15255, #8610, .T. ) ;
#7415 = CYLINDRICAL_SURFACE ( 'NONE', #7076, 5.000000000000004441 ) ;
#7416 = ORIENTED_EDGE ( 'NONE', *, *, #4013, .F. ) ;
#7417 = LINE ( 'NONE', #693, #8397 ) ;
#7418 = VERTEX_POINT ( 'NONE', #3119 ) ;
#7419 = CARTESIAN_POINT ( 'NONE',  ( 27.44407568426044364, 136.8394969516870958, 3.888888888888887063 ) ) ;
#7420 = DIRECTION ( 'NONE',  ( 1.000000000000000000, 0.000000000000000000, 0.000000000000000000 ) ) ;
#7421 = CARTESIAN_POINT ( 'NONE',  ( 13.21952030233119046, 128.8713892059273860, -10.07325499884888664 ) ) ;
#7422 = ORIENTED_EDGE ( 'NONE', *, *, #12197, .F. ) ;
#7423 = DIRECTION ( 'NONE',  ( 1.000000000000000000, 0.000000000000000000, 0.000000000000000000 ) ) ;
#7424 = CARTESIAN_POINT ( 'NONE',  ( 49.99999999999998579, 175.6227766016838245, 5.571800142134975431 ) ) ;
#7425 = CARTESIAN_POINT ( 'NONE',  ( 196.0000000000000000, 187.6227766016837961, 15.00000337241049486 ) ) ;
#7426 = LINE ( 'NONE', #706, #12022 ) ;
#7427 = ORIENTED_EDGE ( 'NONE', *, *, #4947, .F. ) ;
#7428 = EDGE_CURVE ( 'NONE', #4551, #3972, #8518, .T. ) ;
#7429 = EDGE_CURVE ( 'NONE', #10063, #9579, #7368, .T. ) ;
#7430 = EDGE_CURVE ( 'NONE', #7044, #13835, #12769, .T. ) ;
#7431 = ORIENTED_EDGE ( 'NONE', *, *, #15495, .T. ) ;
#7432 = CARTESIAN_POINT ( 'NONE',  ( 21.08563699167523353, 19.99999999999999645, -13.01331479026599602 ) ) ;
#7433 = CARTESIAN_POINT ( 'NONE',  ( 16.17028938446068764, 143.0439382767918346, -16.49999999999050360 ) ) ;
#7434 = ORIENTED_EDGE ( 'NONE', *, *, #680, .F. ) ;
#7435 = FACE_OUTER_BOUND ( 'NONE', #3792, .T. ) ;
#7436 = CARTESIAN_POINT ( 'NONE',  ( 49.99999999999998579, 163.6227766016838530, 10.00000337241049309 ) ) ;
#7437 = ORIENTED_EDGE ( 'NONE', *, *, #10059, .T. ) ;
#7438 = PRODUCT ( 'MirrorLeft Housing Shell', 'MirrorLeft Housing Shell', '', ( #14820 ) ) ;
#7439 = CARTESIAN_POINT ( 'NONE',  ( 196.0000000000000000, 151.6227766016839098, 8.071800142134973655 ) ) ;
#7440 = DIRECTION ( 'NONE',  ( 0.000000000000000000, 0.000000000000000000, 1.000000000000000000 ) ) ;
#7441 = DIRECTION ( 'NONE',  ( 1.000000000000000000, 0.000000000000000000, 0.000000000000000000 ) ) ;
#7442 = CARTESIAN_POINT ( 'NONE',  ( -27.98221281341758626, 18.00000000000000000, 6.321711414556880904 ) ) ;
#7443 = LINE ( 'NONE', #16673, #15394 ) ;
#7444 = DIRECTION ( 'NONE',  ( 1.000000000000000000, 0.000000000000000000, -0.000000000000000000 ) ) ;
#7445 = ORIENTED_EDGE ( 'NONE', *, *, #10983, .T. ) ;
#7446 = FACE_OUTER_BOUND ( 'NONE', #4776, .T. ) ;
#7447 = VERTEX_POINT ( 'NONE', #4708 ) ;
#7448 = DIRECTION ( 'NONE',  ( 0.000000000000000000, 0.000000000000000000, -1.000000000000000000 ) ) ;
#7449 = DIRECTION ( 'NONE',  ( 0.000000000000000000, 1.000000000000000000, 0.000000000000000000 ) ) ;
#7450 = ORIENTED_EDGE ( 'NONE', *, *, #14565, .T. ) ;
#7451 = LINE ( 'NONE', #12688, #6904 ) ;
#7452 = DIRECTION ( 'NONE',  ( 0.000000000000000000, 0.000000000000000000, 1.000000000000000000 ) ) ;
#7453 = EDGE_LOOP ( 'NONE', ( #3337, #14814, #7950, #1742 ) ) ;
#7454 = CONTEXT_DEPENDENT_SHAPE_REPRESENTATION ( #3028, #7295 ) ;
#7455 = LINE ( 'NONE', #742, #4425 ) ;
#7456 = CARTESIAN_POINT ( 'NONE',  ( -83.65340775248648697, 193.1938012187559366, 24.97603563008316385 ) ) ;
#7457 = FACE_OUTER_BOUND ( 'NONE', #4509, .T. ) ;
#7458 = EDGE_CURVE ( 'NONE', #5446, #16788, #640, .T. ) ;
#7459 = DIRECTION ( 'NONE',  ( 0.000000000000000000, -0.8660254037844413721, 0.4999999999999953371 ) ) ;
#7460 = DIRECTION ( 'NONE',  ( 0.000000000000000000, 0.000000000000000000, 1.000000000000000000 ) ) ;
#7461 = EDGE_CURVE ( 'NONE', #7719, #2257, #406, .T. ) ;
#7462 = ORIENTED_EDGE ( 'NONE', *, *, #4402, .T. ) ;
#7463 = DIRECTION ( 'NONE',  ( 0.000000000000000000, 0.000000000000000000, 1.000000000000000000 ) ) ;
#7464 = DIRECTION ( 'NONE',  ( 0.000000000000000000, 0.000000000000000000, -1.000000000000000000 ) ) ;
#7465 = ORIENTED_EDGE ( 'NONE', *, *, #10774, .T. ) ;
#7466 = CARTESIAN_POINT ( 'NONE',  ( -90.33974596215564645, 171.6227766016838245, 0.000000000000000000 ) ) ;
#7467 = CARTESIAN_POINT ( 'NONE',  ( 39.99999999999998579, 4.000000000000007105, 30.00000000000001421 ) ) ;
#7468 = AXIS2_PLACEMENT_3D ( 'NONE', #835, #16862, #13948 ) ;
#7469 = EDGE_LOOP ( 'NONE', ( #4768, #13782 ) ) ;
#7470 = VECTOR ( 'NONE', #13856, 1000.000000000000000 ) ;
#7471 = ORIENTED_EDGE ( 'NONE', *, *, #7710, .T. ) ;
#7472 = VERTEX_POINT ( 'NONE', #6035 ) ;
#7473 = EDGE_CURVE ( 'NONE', #13322, #14130, #11428, .T. ) ;
#7474 = VERTEX_POINT ( 'NONE', #12585 ) ;
#7475 = CARTESIAN_POINT ( 'NONE',  ( 30.00000000000000355, 196.6227766016838245, -35.00000000000000000 ) ) ;
#7476 = ORIENTED_EDGE ( 'NONE', *, *, #5920, .T. ) ;
#7477 = SURFACE_STYLE_USAGE ( .BOTH. , #7313 ) ;
#7478 = CARTESIAN_POINT ( 'NONE',  ( 17.00000000000000000, 171.6227766016838245, 0.000000000000000000 ) ) ;
#7479 = AXIS2_PLACEMENT_3D ( 'NONE', #1450, #5606, #13659 ) ;
#7480 = CARTESIAN_POINT ( 'NONE',  ( 48.00000000000000711, 187.6227766016837961, -10.00000337241049309 ) ) ;
#7481 = LINE ( 'NONE', #6164, #6369 ) ;
#7482 = CIRCLE ( 'NONE', #13135, 5.000000000000000888 ) ;
#7483 = EDGE_CURVE ( 'NONE', #15075, #4396, #10099, .T. ) ;
#7484 = ORIENTED_EDGE ( 'NONE', *, *, #15006, .F. ) ;
#7485 = DIRECTION ( 'NONE',  ( 0.000000000000000000, 0.000000000000000000, 1.000000000000000000 ) ) ;
#7486 = DIRECTION ( 'NONE',  ( 0.000000000000000000, 0.000000000000000000, 1.000000000000000000 ) ) ;
#7487 = LINE ( 'NONE', #10149, #8209 ) ;
#7488 = CARTESIAN_POINT ( 'NONE',  ( -23.66837786580496328, 19.99999999999999645, -17.32703391567687135 ) ) ;
#7489 = CARTESIAN_POINT ( 'NONE',  ( 17.00000000000000000, 191.6227766016837961, -1.224646799147353454E-15 ) ) ;
#7490 = EDGE_CURVE ( 'NONE', #16973, #14936, #5860, .T. ) ;
#7491 = ADVANCED_FACE ( 'NONE', ( #16927 ), #4799, .T. ) ;
#7492 = EDGE_CURVE ( 'NONE', #10900, #5464, #14263, .T. ) ;
#7493 = CYLINDRICAL_SURFACE ( 'NONE', #13015, 1.000000000000000888 ) ;
#7494 = STYLED_ITEM ( 'NONE', ( #1836 ), #11363 ) ;
#7495 = ORIENTED_EDGE ( 'NONE', *, *, #8629, .T. ) ;
#7496 = CARTESIAN_POINT ( 'NONE',  ( -68.00000000000000000, 206.6227766016838245, 2.143131898507868248E-15 ) ) ;
#7497 = AXIS2_PLACEMENT_3D ( 'NONE', #2174, #1016, #3592 ) ;
#7498 = ORIENTED_EDGE ( 'NONE', *, *, #4038, .F. ) ;
#7499 =( LENGTH_UNIT ( ) NAMED_UNIT ( * ) SI_UNIT ( .MILLI., .METRE. ) );
#7500 = CARTESIAN_POINT ( 'NONE',  ( -86.00000000000002842, 146.6227766016838245, -16.00000000000000000 ) ) ;
#7501 = DIRECTION ( 'NONE',  ( -1.000000000000000000, 0.000000000000000000, -8.673617379884037937E-17 ) ) ;
#7502 = ADVANCED_FACE ( 'NONE', ( #13107 ), #13197, .F. ) ;
#7503 = CARTESIAN_POINT ( 'NONE',  ( -40.00000000000000000, 20.00000000000000000, -30.00000000000000355 ) ) ;
#7504 = VECTOR ( 'NONE', #13238, 1000.000000000000000 ) ;
#7505 = ORIENTED_EDGE ( 'NONE', *, *, #2678, .F. ) ;
#7506 = DIRECTION ( 'NONE',  ( 0.000000000000000000, 0.000000000000000000, -1.000000000000000000 ) ) ;
#7507 = DIRECTION ( 'NONE',  ( 0.000000000000000000, 0.000000000000000000, 1.000000000000000000 ) ) ;
#7508 = VECTOR ( 'NONE', #13077, 1000.000000000000000 ) ;
#7509 = DIRECTION ( 'NONE',  ( 1.000000000000000000, 0.000000000000000000, -0.000000000000000000 ) ) ;
#7510 = CARTESIAN_POINT ( 'NONE',  ( 29.74498994719569467, 202.6234830987602038, -16.24672887513766639 ) ) ;
#7511 = ORIENTED_EDGE ( 'NONE', *, *, #3064, .T. ) ;
#7512 = ORIENTED_EDGE ( 'NONE', *, *, #2532, .F. ) ;
#7513 = CARTESIAN_POINT ( 'NONE',  ( 18.45742352454476887, 29.95282391178955095, -14.36414658362611974 ) ) ;
#7514 = CARTESIAN_POINT ( 'NONE',  ( 27.42718951882975631, 138.9142741377072525, -4.446260193316556197 ) ) ;
#7515 = VERTEX_POINT ( 'NONE', #11864 ) ;
#7516 = CYLINDRICAL_SURFACE ( 'NONE', #5564, 5.000000000000000888 ) ;
#7517 = VECTOR ( 'NONE', #4884, 1000.000000000000000 ) ;
#7518 = DIRECTION ( 'NONE',  ( -1.000000000000000000, -0.000000000000000000, -0.000000000000000000 ) ) ;
#7519 = AXIS2_PLACEMENT_3D ( 'NONE', #9222, #14372, #12957 ) ;
#7520 = ORIENTED_EDGE ( 'NONE', *, *, #1052, .F. ) ;
#7521 = VECTOR ( 'NONE', #4902, 1000.000000000000000 ) ;
#7522 = FACE_BOUND ( 'NONE', #11451, .T. ) ;
#7523 = ADVANCED_FACE ( 'NONE', ( #5053 ), #9117, .F. ) ;
#7524 = EDGE_CURVE ( 'NONE', #10721, #15996, #7362, .T. ) ;
#7525 = EDGE_CURVE ( 'NONE', #4295, #9729, #6312, .T. ) ;
#7526 = CYLINDRICAL_SURFACE ( 'NONE', #7805, 2.499999999999998668 ) ;
#7527 = DIRECTION ( 'NONE',  ( 0.000000000000000000, 0.000000000000000000, 1.000000000000000000 ) ) ;
#7528 = CARTESIAN_POINT ( 'NONE',  ( -13.45813206906208848, 31.92660440999782523, 10.88283926110020516 ) ) ;
#7529 = DIRECTION ( 'NONE',  ( -1.000000000000000000, 0.000000000000000000, 0.000000000000000000 ) ) ;
#7530 = AXIS2_PLACEMENT_3D ( 'NONE', #8767, #5845, #12925 ) ;
#7531 = LINE ( 'NONE', #11770, #1273 ) ;
#7532 = VECTOR ( 'NONE', #8248, 1000.000000000000000 ) ;
#7533 = ORIENTED_EDGE ( 'NONE', *, *, #4116, .T. ) ;
#7534 = DIRECTION ( 'NONE',  ( 0.000000000000000000, -0.8660254037844413721, -0.4999999999999953371 ) ) ;
#7535 = AXIS2_PLACEMENT_3D ( 'NONE', #10445, #3906, #9292 ) ;
#7536 = ORIENTED_EDGE ( 'NONE', *, *, #2566, .T. ) ;
#7537 = PRESENTATION_LAYER_ASSIGNMENT (  '', '', ( #5282 ) ) ;
#7538 = DIRECTION ( 'NONE',  ( 1.000000000000000000, 0.000000000000000000, 0.000000000000000000 ) ) ;
#7539 = CIRCLE ( 'NONE', #15738, 5.999999999999998224 ) ;
#7540 = CARTESIAN_POINT ( 'NONE',  ( -32.65879391391307252, 118.8520289717560843, 4.574240649589675911 ) ) ;
#7541 = ORIENTED_EDGE ( 'NONE', *, *, #6579, .F. ) ;
#7542 = DIRECTION ( 'NONE',  ( -1.000000000000000000, -0.000000000000000000, -0.000000000000000000 ) ) ;
#7543 = CARTESIAN_POINT ( 'NONE',  ( 22.52789404479186786, 20.00000000000113687, 11.66574595783169954 ) ) ;
#7544 = ORIENTED_EDGE ( 'NONE', *, *, #8256, .T. ) ;
#7545 = EDGE_CURVE ( 'NONE', #919, #6279, #815, .T. ) ;
#7546 = VECTOR ( 'NONE', #16213, 1000.000000000000000 ) ;
#7547 = PRESENTATION_LAYER_ASSIGNMENT (  '', '', ( #8396 ) ) ;
#7548 = CARTESIAN_POINT ( 'NONE',  ( 15.00000000000000000, 143.1210915093834330, 16.64102305613075572 ) ) ;
#7549 = CARTESIAN_POINT ( 'NONE',  ( 32.79368516360896280, 189.6403081819231886, -27.64877209012309223 ) ) ;
#7550 = CARTESIAN_POINT ( 'NONE',  ( -11.03695849842137910, 30.81357570984703642, -14.42948753805835871 ) ) ;
#7551 = CYLINDRICAL_SURFACE ( 'NONE', #773, 2.000000000000001776 ) ;
#7552 = DIRECTION ( 'NONE',  ( 1.000000000000000000, -0.000000000000000000, -0.000000000000000000 ) ) ;
#7553 = VERTEX_POINT ( 'NONE', #13030 ) ;
#7554 = LINE ( 'NONE', #10287, #1082 ) ;
#7555 = CARTESIAN_POINT ( 'NONE',  ( -20.85266279178580362, 19.99999999999999645, -20.15433268689462665 ) ) ;
#7556 = ORIENTED_EDGE ( 'NONE', *, *, #2108, .T. ) ;
#7557 = CARTESIAN_POINT ( 'NONE',  ( -206.8260782938593820, 174.6444607475611406, -3.997336900281264427 ) ) ;
#7558 = DIRECTION ( 'NONE',  ( 1.000000000000000000, 0.000000000000000000, 0.000000000000000000 ) ) ;
#7559 = ORIENTED_EDGE ( 'NONE', *, *, #5476, .F. ) ;
#7560 = CIRCLE ( 'NONE', #15764, 740.0000000000000000 ) ;
#7561 = ORIENTED_EDGE ( 'NONE', *, *, #15602, .T. ) ;
#7562 = ORIENTED_EDGE ( 'NONE', *, *, #14110, .F. ) ;
#7563 = CARTESIAN_POINT ( 'NONE',  ( 16.24385689529520604, 136.8350826111700655, -4.682368943704262598 ) ) ;
#7564 = CIRCLE ( 'NONE', #15478, 2.500000000000000000 ) ;
#7565 = EDGE_CURVE ( 'NONE', #3708, #10702, #6645, .T. ) ;
#7566 = DIRECTION ( 'NONE',  ( -1.000000000000000000, -0.000000000000000000, -0.000000000000000000 ) ) ;
#7567 = ORIENTED_EDGE ( 'NONE', *, *, #9265, .F. ) ;
#7568 = CARTESIAN_POINT ( 'NONE',  ( -50.00000000000000000, 171.6227766016838245, 19.49999999999998934 ) ) ;
#7569 = DIRECTION ( 'NONE',  ( 1.000000000000000000, 0.000000000000000000, 0.000000000000000000 ) ) ;
#7570 = CARTESIAN_POINT ( 'NONE',  ( 22.88332935572807969, 29.84310215611307271, 6.048604702147989620 ) ) ;
#7571 = CARTESIAN_POINT ( 'NONE',  ( -43.00000000000000000, 140.0000000000000000, 0.000000000000000000 ) ) ;
#7572 = CIRCLE ( 'NONE', #4755, 2.500000000000002220 ) ;
#7573 = AXIS2_PLACEMENT_3D ( 'NONE', #14782, #1152, #14866 ) ;
#7574 = COLOUR_RGB ( '', 0.09019608, 0.27058824, 0.51372549) ;
#7575 = EDGE_LOOP ( 'NONE', ( #1523, #2859, #16822 ) ) ;
#7576 = CARTESIAN_POINT ( 'NONE',  ( 49.99999999999998579, 171.6227766016838245, -12.50000337241049131 ) ) ;
#7577 = DIRECTION ( 'NONE',  ( 0.000000000000000000, 0.000000000000000000, -1.000000000000000000 ) ) ;
#7578 = DIRECTION ( 'NONE',  ( 0.000000000000000000, 0.000000000000000000, 1.000000000000000000 ) ) ;
#7579 = CARTESIAN_POINT ( 'NONE',  ( -15.33310217279680288, 19.99999999999999645, -4.999999999999999112 ) ) ;
#7580 = DIRECTION ( 'NONE',  ( -1.000000000000000000, -0.000000000000000000, -0.000000000000000000 ) ) ;
#7581 = CARTESIAN_POINT ( 'NONE',  ( 30.56782666082448330, 201.5917424073649613, 13.81529814621278085 ) ) ;
#7582 = AXIS2_PLACEMENT_3D ( 'NONE', #8857, #16839, #15770 ) ;
#7583 = VERTEX_POINT ( 'NONE', #15670 ) ;
#7584 = EDGE_CURVE ( 'NONE', #3061, #6774, #133, .T. ) ;
#7585 = FACE_BOUND ( 'NONE', #14911, .T. ) ;
#7587 = LINE ( 'NONE', #3518, #16113 ) ;
#7586 = CIRCLE ( 'NONE', #14381, 30.00000000000000000 ) ;
#7588 = ORIENTED_EDGE ( 'NONE', *, *, #9562, .F. ) ;
#7589 = CARTESIAN_POINT ( 'NONE',  ( 27.44407568426044008, 126.9014170516880284, 4.999999999999997335 ) ) ;
#7590 = DIRECTION ( 'NONE',  ( 1.000000000000000000, 0.000000000000000000, -0.000000000000000000 ) ) ;
#7591 = EDGE_CURVE ( 'NONE', #10629, #8608, #13415, .T. ) ;
#7592 = CARTESIAN_POINT ( 'NONE',  ( -24.99999999999999289, 90.00000000000000000, 4.999999999999999112 ) ) ;
#7593 = ADVANCED_FACE ( 'NONE', ( #6374 ), #15666, .F. ) ;
#7594 = ORIENTED_EDGE ( 'NONE', *, *, #11549, .T. ) ;
#7595 = DIRECTION ( 'NONE',  ( -0.000000000000000000, -0.000000000000000000, 1.000000000000000000 ) ) ;
#7596 = AXIS2_PLACEMENT_3D ( 'NONE', #13196, #2585, #5145 ) ;
#7597 = FACE_OUTER_BOUND ( 'NONE', #13495, .T. ) ;
#7598 = VECTOR ( 'NONE', #12071, 1000.000000000000000 ) ;
#7599 = DIRECTION ( 'NONE',  ( 0.000000000000000000, 0.8660254037844413721, 0.4999999999999952816 ) ) ;
#7600 = CARTESIAN_POINT ( 'NONE',  ( 39.99999999999998579, 4.000000000000007994, 33.00000000000001421 ) ) ;
#7601 = EDGE_LOOP ( 'NONE', ( #14739, #6534, #15227, #4634 ) ) ;
#7602 = EDGE_LOOP ( 'NONE', ( #1275, #15487, #1713, #7768 ) ) ;
#7603 = CARTESIAN_POINT ( 'NONE',  ( 17.69056612348262192, 19.99999999999999645, -14.65191630173004711 ) ) ;
#7604 = DIRECTION ( 'NONE',  ( 0.000000000000000000, 0.000000000000000000, 1.000000000000000000 ) ) ;
#7605 = ORIENTED_EDGE ( 'NONE', *, *, #10394, .F. ) ;
#7606 = DIRECTION ( 'NONE',  ( 1.000000000000000000, 0.000000000000000000, 0.000000000000000000 ) ) ;
#7607 = CARTESIAN_POINT ( 'NONE',  ( 39.99999999999998579, -20.00000000000000000, -40.00000000000001421 ) ) ;
#7608 = AXIS2_PLACEMENT_3D ( 'NONE', #4412, #1753, #5651 ) ;
#7609 = ORIENTED_EDGE ( 'NONE', *, *, #2631, .F. ) ;
#7610 = CIRCLE ( 'NONE', #15249, 248.0000000000000000 ) ;
#7611 = CARTESIAN_POINT ( 'NONE',  ( 30.00000000000000355, 196.6227766016838245, -16.00000000000000000 ) ) ;
#7612 = PRODUCT_DEFINITION ( 'UNKNOWN', '', #11787, #2886 ) ;
#7613 = CARTESIAN_POINT ( 'NONE',  ( 196.0000000000000000, 175.6227766016838245, -5.571800142134975431 ) ) ;
#7614 = CARTESIAN_POINT ( 'NONE',  ( 27.75000000000000000, 0.000000000000000000, 0.000000000000000000 ) ) ;
#7615 = CARTESIAN_POINT ( 'NONE',  ( -12.63609539511579527, 18.00000000000000000, 24.35132453916584794 ) ) ;
#7616 = DIRECTION ( 'NONE',  ( 0.000000000000000000, 0.000000000000000000, -1.000000000000000000 ) ) ;
#7617 = CARTESIAN_POINT ( 'NONE',  ( 30.54126313378810664, 140.6457587561385196, -16.29186131275297811 ) ) ;
#7618 = ORIENTED_EDGE ( 'NONE', *, *, #250, .T. ) ;
#7619 = DIRECTION ( 'NONE',  ( 0.000000000000000000, -0.4999999999999952816, 0.8660254037844413721 ) ) ;
#7620 = AXIS2_PLACEMENT_3D ( 'NONE', #10332, #2198, #7599 ) ;
#7621 = ORIENTED_EDGE ( 'NONE', *, *, #14742, .F. ) ;
#7622 = CARTESIAN_POINT ( 'NONE',  ( 0.000000000000000000, -1.732050807568885631, 0.000000000000000000 ) ) ;
#7623 = AXIS2_PLACEMENT_3D ( 'NONE', #3780, #15824, #3611 ) ;
#7624 = CARTESIAN_POINT ( 'NONE',  ( 24.00000000000000000, 146.6227766016838245, -16.00000000000000000 ) ) ;
#7625 = ADVANCED_FACE ( 'NONE', ( #17012 ), #2220, .T. ) ;
#7626 = ORIENTED_EDGE ( 'NONE', *, *, #575, .T. ) ;
#7627 = CARTESIAN_POINT ( 'NONE',  ( 48.00000000000000711, 183.6227766016837961, 8.071800142134975431 ) ) ;
#7628 = DIRECTION ( 'NONE',  ( 0.000000000000000000, -0.000000000000000000, -1.000000000000000000 ) ) ;
#7629 = CARTESIAN_POINT ( 'NONE',  ( 22.45383620668762248, 29.90040889522806111, 11.60055593449971845 ) ) ;
#7630 = VECTOR ( 'NONE', #4506, 1000.000000000000000 ) ;
#7631 = AXIS2_PLACEMENT_3D ( 'NONE', #5539, #1386, #2799 ) ;
#7632 = EDGE_LOOP ( 'NONE', ( #6921, #10128, #16246 ) ) ;
#7633 = AXIS2_PLACEMENT_3D ( 'NONE', #12108, #10779, #4058 ) ;
#7634 = CARTESIAN_POINT ( 'NONE',  ( -68.00000000000000000, 171.6227766016838245, 0.000000000000000000 ) ) ;
#7635 = CARTESIAN_POINT ( 'NONE',  ( -100.0000000000000000, 171.6227766016838245, 0.000000000000000000 ) ) ;
#7636 = PLANE ( 'NONE',  #8231 ) ;
#7637 = CARTESIAN_POINT ( 'NONE',  ( -16.30611068361784532, 32.76923076923076650, -4.999999999999998224 ) ) ;
#7638 = ORIENTED_EDGE ( 'NONE', *, *, #9868, .T. ) ;
#7639 = FACE_OUTER_BOUND ( 'NONE', #7305, .T. ) ;
#7640 = ORIENTED_EDGE ( 'NONE', *, *, #16047, .F. ) ;
#7641 = CARTESIAN_POINT ( 'NONE',  ( 24.44329345585415325, 194.3322840258869064, -26.63593000238176955 ) ) ;
#7642 = DIRECTION ( 'NONE',  ( 0.000000000000000000, 0.000000000000000000, 1.000000000000000000 ) ) ;
#7643 = AXIS2_PLACEMENT_3D ( 'NONE', #1735, #9777, #11189 ) ;
#7644 = ADVANCED_FACE ( 'NONE', ( #11769 ), #17180, .T. ) ;
#7645 = ORIENTED_EDGE ( 'NONE', *, *, #4820, .F. ) ;
#7646 = ADVANCED_FACE ( 'NONE', ( #4878 ), #15765, .F. ) ;
#7647 = ORIENTED_EDGE ( 'NONE', *, *, #4565, .T. ) ;
#7648 = EDGE_CURVE ( 'NONE', #4086, #15544, #6913, .T. ) ;
#7649 = ORIENTED_EDGE ( 'NONE', *, *, #2366, .T. ) ;
#7650 = CIRCLE ( 'NONE', #12189, 2.499999999999998668 ) ;
#7651 = CARTESIAN_POINT ( 'NONE',  ( -81.13499951972124791, 154.0589040539455539, -27.93804624201381515 ) ) ;
#7652 = ORIENTED_EDGE ( 'NONE', *, *, #4400, .F. ) ;
#7653 = DIRECTION ( 'NONE',  ( 1.000000000000000000, 0.000000000000000000, 0.000000000000000000 ) ) ;
#7654 = CARTESIAN_POINT ( 'NONE',  ( -8.461393309425545795, 30.35704578695612099, 12.95687587100684368 ) ) ;
#7655 = CARTESIAN_POINT ( 'NONE',  ( -17.63576980228536328, 32.18555361985414720, 8.400096275226864861 ) ) ;
#7656 = CARTESIAN_POINT ( 'NONE',  ( 24.22132560812392299, 148.2463666031633807, -26.04982723689807500 ) ) ;
#7657 = VECTOR ( 'NONE', #13946, 1000.000000000000000 ) ;
#7658 = CARTESIAN_POINT ( 'NONE',  ( 34.93420767782698988, 18.00000000000000000, 6.321724734778991106 ) ) ;
#7659 = DIRECTION ( 'NONE',  ( -1.000000000000000000, -0.000000000000000000, -0.000000000000000000 ) ) ;
#7660 = ORIENTED_EDGE ( 'NONE', *, *, #17290, .F. ) ;
#7661 = DIRECTION ( 'NONE',  ( -0.000000000000000000, -0.000000000000000000, -1.000000000000000000 ) ) ;
#7662 = CARTESIAN_POINT ( 'NONE',  ( 17.21487247493544714, 29.96934980803111159, -14.74175109707249831 ) ) ;
#7663 = CARTESIAN_POINT ( 'NONE',  ( -20.49999999999998224, 10.00000000000000000, -28.00000000000000355 ) ) ;
#7664 = ADVANCED_FACE ( 'NONE', ( #11953 ), #5227, .F. ) ;
#7665 = CARTESIAN_POINT ( 'NONE',  ( 24.93507336697353338, 29.86842105263157521, 5.660390792616599498 ) ) ;
#7666 = ORIENTED_EDGE ( 'NONE', *, *, #720, .F. ) ;
#7667 = CARTESIAN_POINT ( 'NONE',  ( -48.00000000000000000, 171.6227766016838245, -20.00000000000000355 ) ) ;
#7668 = VECTOR ( 'NONE', #5432, 1000.000000000000000 ) ;
#7669 = CARTESIAN_POINT ( 'NONE',  ( 31.52313204192882523, 201.3896308033654634, 14.24607874381217520 ) ) ;
#7670 = ORIENTED_EDGE ( 'NONE', *, *, #5964, .F. ) ;
#7671 = CARTESIAN_POINT ( 'NONE',  ( -32.02886766642249228, 100.0581520846466645, -5.500000000000001776 ) ) ;
#7672 = DIRECTION ( 'NONE',  ( 0.000000000000000000, 0.000000000000000000, 1.000000000000000000 ) ) ;
#7673 = ORIENTED_EDGE ( 'NONE', *, *, #9928, .T. ) ;
#7674 = CARTESIAN_POINT ( 'NONE',  ( -77.05212259621265503, 142.5723011982437072, 15.66001370690270633 ) ) ;
#7675 = CARTESIAN_POINT ( 'NONE',  ( 17.01529014380724192, 17.99999999999885958, -12.76845467807931733 ) ) ;
#7676 = PLANE ( 'NONE',  #10699 ) ;
#7677 = CARTESIAN_POINT ( 'NONE',  ( 6.803110712587624676, 134.0269829078799262, -12.98040381008119759 ) ) ;
#7678 = EDGE_LOOP ( 'NONE', ( #5537, #10886, #3508, #4604 ) ) ;
#7679 = DIRECTION ( 'NONE',  ( -1.000000000000000000, 0.000000000000000000, 0.000000000000000000 ) ) ;
#7680 = DIRECTION ( 'NONE',  ( -1.000000000000000000, -0.000000000000000000, -0.000000000000000000 ) ) ;
#7681 = EDGE_CURVE ( 'NONE', #3017, #1185, #11437, .T. ) ;
#7682 = DIRECTION ( 'NONE',  ( -1.000000000000000000, 0.000000000000000000, 0.000000000000000000 ) ) ;
#7683 = EDGE_CURVE ( 'NONE', #8077, #6189, #12298, .T. ) ;
#7684 = CARTESIAN_POINT ( 'NONE',  ( 24.00000000000000000, 196.6227766016838245, -24.49489742783178770 ) ) ;
#7685 = ORIENTED_EDGE ( 'NONE', *, *, #3936, .T. ) ;
#7686 = ORIENTED_EDGE ( 'NONE', *, *, #3503, .F. ) ;
#7687 = CARTESIAN_POINT ( 'NONE',  ( 20.11141720500585350, 19.99999999999999645, -24.32074799214527516 ) ) ;
#7688 = CARTESIAN_POINT ( 'NONE',  ( 40.00000000000000711, 196.6227766016838245, 0.000000000000000000 ) ) ;
#7689 = EDGE_LOOP ( 'NONE', ( #1272, #16118, #5776, #10557, #9882, #10249, #800, #6290, #3618, #5462, #6200, #13293, #7350, #10544 ) ) ;
#7690 = CARTESIAN_POINT ( 'NONE',  ( -100.0000000000000000, 136.6227766016838245, 0.000000000000000000 ) ) ;
#7691 = EDGE_CURVE ( 'NONE', #5007, #13962, #2753, .T. ) ;
#7692 = CARTESIAN_POINT ( 'NONE',  ( 14.46714703242257904, 138.5709836085849531, -4.391619799165513705 ) ) ;
#7693 = EDGE_CURVE ( 'NONE', #9063, #1055, #9387, .T. ) ;
#7694 = VERTEX_POINT ( 'NONE', #13555 ) ;
#7695 = DIRECTION ( 'NONE',  ( 0.000000000000000000, 0.000000000000000000, 1.000000000000000000 ) ) ;
#7696 = LINE ( 'NONE', #15262, #16149 ) ;
#7697 = CARTESIAN_POINT ( 'NONE',  ( 39.99999999999999289, 20.00000000000000000, 0.000000000000000000 ) ) ;
#7698 = LINE ( 'NONE', #15937, #2691 ) ;
#7699 = CARTESIAN_POINT ( 'NONE',  ( -11.31385407355777950, 31.26810920821015216, 12.21116371260378308 ) ) ;
#7700 = B_SPLINE_CURVE_WITH_KNOTS ( 'NONE', 3,
 ( #1915, #14221, #1826, #4837, #7141, #14143, #4659, #10044, #2083, #15458 ),
 .UNSPECIFIED., .F., .F.,
 ( 4, 2, 2, 2, 4 ),
 ( 0.03775390620236026423, 0.04033669301524706735, 0.04291947982813386353, 0.04550226664102066665, 0.04808505345390746977 ),
 .UNSPECIFIED. ) ;
#7701 = DIRECTION ( 'NONE',  ( -1.000000000000000000, 0.000000000000000000, 0.000000000000000000 ) ) ;
#7702 = CARTESIAN_POINT ( 'NONE',  ( -151.9615242270660929, 171.6227766016838245, 0.000000000000000000 ) ) ;
#7703 = ORIENTED_EDGE ( 'NONE', *, *, #7337, .F. ) ;
#7704 = CARTESIAN_POINT ( 'NONE',  ( 196.0000000000000000, 151.6227766016839098, 5.571800142134973655 ) ) ;
#7705 = ORIENTED_EDGE ( 'NONE', *, *, #5497, .T. ) ;
#7706 = CARTESIAN_POINT ( 'NONE',  ( -138.7106781186547266, 171.6227766016838245, -2.602085213965210642E-15 ) ) ;
#7707 = PLANE ( 'NONE',  #8663 ) ;
#7708 = ORIENTED_EDGE ( 'NONE', *, *, #3478, .F. ) ;
#7709 = DIRECTION ( 'NONE',  ( -1.000000000000000000, -0.000000000000000000, 0.000000000000000000 ) ) ;
#7710 = EDGE_CURVE ( 'NONE', #14757, #7241, #12139, .T. ) ;
#7711 = CARTESIAN_POINT ( 'NONE',  ( 15.22098041563561388, 126.0279773824920824, 6.884464680362713196 ) ) ;
#7712 = CARTESIAN_POINT ( 'NONE',  ( 22.95484754400920124, 19.99999999999884537, 11.15425480658508306 ) ) ;
#7713 = ORIENTED_EDGE ( 'NONE', *, *, #8581, .T. ) ;
#7714 = CARTESIAN_POINT ( 'NONE',  ( -80.00000000000002842, 146.6227766016838245, 0.000000000000000000 ) ) ;
#7715 = LINE ( 'NONE', #17292, #16940 ) ;
#7716 = CARTESIAN_POINT ( 'NONE',  ( -12.61248932541308676, 31.15232071419451643, -13.80069170922183375 ) ) ;
#7717 = ADVANCED_FACE ( 'NONE', ( #175, #12221 ), #1429, .T. ) ;
#7718 = CARTESIAN_POINT ( 'NONE',  ( -10.50630597522742171, 31.01369813559846378, -12.50559288035636563 ) ) ;
#7719 = VERTEX_POINT ( 'NONE', #6900 ) ;
#7720 = CARTESIAN_POINT ( 'NONE',  ( -50.00000000000005684, 8.000000000000000000, 35.00000000000000711 ) ) ;
#7721 = ORIENTED_EDGE ( 'NONE', *, *, #11731, .F. ) ;
#7722 = CARTESIAN_POINT ( 'NONE',  ( 29.09601211296537571, 190.6868548533384455, -29.35237411376976269 ) ) ;
#7723 = DIRECTION ( 'NONE',  ( 0.000000000000000000, 0.000000000000000000, 1.000000000000000000 ) ) ;
#7724 = EDGE_LOOP ( 'NONE', ( #10611, #7422 ) ) ;
#7725 = VERTEX_POINT ( 'NONE', #14708 ) ;
#7726 = ORIENTED_EDGE ( 'NONE', *, *, #14841, .F. ) ;
#7727 = B_SPLINE_CURVE_WITH_KNOTS ( 'NONE', 3,
 ( #11899, #3953, #7654, #3856, #9245, #3588, #6414, #1108, #13064, #2169, #14297, #855, #2341, #9068, #17308, #5262, #15891, #6246, #3682, #2259, #5176, #10567 ),
 .UNSPECIFIED., .F., .F.,
 ( 4, 2, 2, 2, 2, 2, 2, 2, 2, 2, 4 ),
 ( 0.000000000000000000, 0.001700754388868652408, 0.003401508777737304815, 0.005102263166605957440, 0.005952640361040282234, 0.006803017555474607028, 0.008503771944343253147, 0.01020452633321189927, 0.01190528072208054712, 0.01275565791651486931, 0.01360603511094918977 ),
 .UNSPECIFIED. ) ;
#7728 = CARTESIAN_POINT ( 'NONE',  ( -87.25061104762463060, 148.5880153409831905, -23.63707964515040416 ) ) ;
#7729 = ORIENTED_EDGE ( 'NONE', *, *, #14504, .T. ) ;
#7730 = CARTESIAN_POINT ( 'NONE',  ( 0.000000000000000000, 0.000000000000000000, 0.000000000000000000 ) ) ;
#7731 = CARTESIAN_POINT ( 'NONE',  ( -98.00000000000000000, 171.6227766016838245, 5.000000000000006217 ) ) ;
#7732 = CARTESIAN_POINT ( 'NONE',  ( -11.99846793330598693, 31.02137248309377071, 14.08482506821421509 ) ) ;
#7733 = CARTESIAN_POINT ( 'NONE',  ( 28.19759474139298305, 152.3499437555877876, -29.21584945930381494 ) ) ;
#7734 = EDGE_CURVE ( 'NONE', #16797, #3065, #11870, .T. ) ;
#7735 = CARTESIAN_POINT ( 'NONE',  ( 22.93524650466135739, 29.84210526317653489, 5.528689893908154573 ) ) ;
#7736 = EDGE_CURVE ( 'NONE', #14104, #11995, #6213, .T. ) ;
#7737 = CARTESIAN_POINT ( 'NONE',  ( 40.00000000000000711, 196.6227766016838245, 0.000000000000000000 ) ) ;
#7738 = EDGE_CURVE ( 'NONE', #9579, #8740, #12434, .T. ) ;
#7739 = ORIENTED_EDGE ( 'NONE', *, *, #16359, .T. ) ;
#7740 = CARTESIAN_POINT ( 'NONE',  ( 19.59022622986824302, 142.1737554346910599, 14.89790021284453303 ) ) ;
#7741 = DIRECTION ( 'NONE',  ( 1.000000000000000000, 0.000000000000000000, 0.000000000000000000 ) ) ;
#7743 = CARTESIAN_POINT ( 'NONE',  ( -15.00000000000002665, 130.0000000000000000, -15.00000000000000000 ) ) ;
#7742 = AXIS2_PLACEMENT_3D ( 'NONE', #10109, #14198, #826 ) ;
#7744 = DIRECTION ( 'NONE',  ( 0.000000000000000000, 0.000000000000000000, -1.000000000000000000 ) ) ;
#7745 = CARTESIAN_POINT ( 'NONE',  ( 23.61565302391275267, 29.88537503463918554, 10.00682404417760551 ) ) ;
#7746 = ORIENTED_EDGE ( 'NONE', *, *, #7683, .T. ) ;
#7747 = LINE ( 'NONE', #12003, #13159 ) ;
#7748 = CARTESIAN_POINT ( 'NONE',  ( -195.2299705378136991, 173.3300053194287784, -3.811055608065186728 ) ) ;
#7749 = EDGE_LOOP ( 'NONE', ( #7984, #9500, #15376, #14398 ) ) ;
#7750 = CARTESIAN_POINT ( 'NONE',  ( -23.00000000000000000, 120.0000000000000426, -15.00000000000000000 ) ) ;
#7751 = AXIS2_PLACEMENT_3D ( 'NONE', #6209, #9033, #7616 ) ;
#7752 = AXIS2_PLACEMENT_3D ( 'NONE', #10677, #9348, #15010 ) ;
#7753 = VERTEX_POINT ( 'NONE', #5415 ) ;
#7754 = CARTESIAN_POINT ( 'NONE',  ( -82.07464743585514100, 142.0696621759509810, 14.68466941333284126 ) ) ;
#7755 = VECTOR ( 'NONE', #10576, 1000.000000000000000 ) ;
#7756 = CARTESIAN_POINT ( 'NONE',  ( 15.97392895077415531, 29.97895215653467815, -12.94942366938410139 ) ) ;
#7757 = CARTESIAN_POINT ( 'NONE',  ( -82.59785185926696727, 141.2103550623191381, -17.32402235562967618 ) ) ;
#7758 = CARTESIAN_POINT ( 'NONE',  ( -208.0000000000000853, 170.0678595944000620, -2.693195258168412654 ) ) ;
#7759 = ORIENTED_EDGE ( 'NONE', *, *, #2696, .T. ) ;
#7760 = FACE_OUTER_BOUND ( 'NONE', #14481, .T. ) ;
#7761 = DIRECTION ( 'NONE',  ( -1.000000000000000000, 0.000000000000000000, 0.000000000000000000 ) ) ;
#7762 = DIRECTION ( 'NONE',  ( -1.000000000000000000, 0.000000000000000000, 0.000000000000000000 ) ) ;
#7763 = FILL_AREA_STYLE_COLOUR ( '', #2706 ) ;
#7764 = CIRCLE ( 'NONE', #6928, 5.000000000000000888 ) ;
#7765 = CIRCLE ( 'NONE', #16832, 5.000000000000000888 ) ;
#7766 = ORIENTED_EDGE ( 'NONE', *, *, #7405, .F. ) ;
#7767 = CIRCLE ( 'NONE', #10318, 5.000000000000000888 ) ;
#7768 = ORIENTED_EDGE ( 'NONE', *, *, #8316, .T. ) ;
#7769 = CARTESIAN_POINT ( 'NONE',  ( 12.56741672263968290, 142.0153054307823481, -18.66563201629009328 ) ) ;
#7770 = ORIENTED_EDGE ( 'NONE', *, *, #2304, .T. ) ;
#7771 = LINE ( 'NONE', #6457, #6128 ) ;
#7772 = CARTESIAN_POINT ( 'NONE',  ( 12.31199832339570577, 129.9194306174879046, -10.85217099066659685 ) ) ;
#7773 = EDGE_LOOP ( 'NONE', ( #6309, #6635, #12971, #13650 ) ) ;
#7774 = DIRECTION ( 'NONE',  ( 1.000000000000000000, 0.000000000000000000, 0.000000000000000000 ) ) ;
#7775 = CARTESIAN_POINT ( 'NONE',  ( -45.00000000000000711, -20.00000000000000000, 40.00000000000000711 ) ) ;
#7776 = ADVANCED_FACE ( 'NONE', ( #10805 ), #4008, .F. ) ;
#7777 = AXIS2_PLACEMENT_3D ( 'NONE', #9270, #15998, #9090 ) ;
#7778 = CARTESIAN_POINT ( 'NONE',  ( -87.50000000000004263, 196.6227766016838245, -21.54065922853802562 ) ) ;
#7779 = COLOUR_RGB ( '', 0.31764706, 0.68627451, 0.89019608) ;
#7780 = CARTESIAN_POINT ( 'NONE',  ( 33.65098944192141772, 193.2024116766813222, 24.96685975555417514 ) ) ;
#7781 = DIRECTION ( 'NONE',  ( 0.000000000000000000, 0.000000000000000000, -1.000000000000000000 ) ) ;
#7782 = CARTESIAN_POINT ( 'NONE',  ( 196.0000000000000000, 171.6227766016838245, 10.00000337241048953 ) ) ;
#7783 = CIRCLE ( 'NONE', #1290, 5.000000000000018652 ) ;
#7784 = CARTESIAN_POINT ( 'NONE',  ( 196.0000000000000000, 151.6227766016839098, -5.571800142134973655 ) ) ;
#7785 = DIRECTION ( 'NONE',  ( -1.000000000000000000, 0.000000000000000000, 0.000000000000000000 ) ) ;
#7786 = CARTESIAN_POINT ( 'NONE',  ( 33.16115143954747424, 141.5060039278119177, -17.83622402891603187 ) ) ;
#7787 = ORIENTED_EDGE ( 'NONE', *, *, #11965, .T. ) ;
#7788 = CYLINDRICAL_SURFACE ( 'NONE', #531, 2.500000000000000444 ) ;
#7789 = ORIENTED_EDGE ( 'NONE', *, *, #15984, .T. ) ;
#7790 = CARTESIAN_POINT ( 'NONE',  ( 37.99999999999999289, 2.000000000000000000, 8.789265611615818404E-15 ) ) ;
#7791 = VECTOR ( 'NONE', #12592, 1000.000000000000000 ) ;
#7792 = AXIS2_PLACEMENT_3D ( 'NONE', #11445, #16943, #3314 ) ;
#7793 = B_SPLINE_CURVE_WITH_KNOTS ( 'NONE', 3,
 ( #16171, #5531, #12258, #15079, #3044, #6942, #14824, #130, #9505, #2956, #8092, #12347, #8446, #13508, #13598, #15000, #8269, #221, #1468, #12439, #10922, #1639, #13770 ),
 .UNSPECIFIED., .F., .F.,
 ( 4, 2, 2, 2, 2, 2, 2, 2, 1, 2, 2, 4 ),
 ( 0.000000000000000000, 0.001562580732212274365, 0.002343871098318411547, 0.003125161464424548730, 0.004687742196636830901, 0.006250322928849113939, 0.007812903661061397845, 0.008594194027167533292, 0.009375484393273670475, 0.01015677475937980939, 0.01093806512548594484, 0.01250064585769823135 ),
 .UNSPECIFIED. ) ;
#7794 = PLANE ( 'NONE',  #2161 ) ;
#7795 = AXIS2_PLACEMENT_3D ( 'NONE', #5169, #17380, #11798 ) ;
#7796 = VERTEX_POINT ( 'NONE', #5491 ) ;
#7797 = DIRECTION ( 'NONE',  ( -1.000000000000000000, 0.000000000000000000, 0.000000000000000000 ) ) ;
#7798 = CARTESIAN_POINT ( 'NONE',  ( 14.44088586081352688, 138.6571688462224472, 6.678806037552732278 ) ) ;
#7799 = EDGE_LOOP ( 'NONE', ( #4092, #7626, #2755, #16409 ) ) ;
#7800 = PLANE ( 'NONE',  #5364 ) ;
#7801 = EDGE_CURVE ( 'NONE', #4462, #3385, #9037, .T. ) ;
#7802 = ORIENTED_EDGE ( 'NONE', *, *, #628, .F. ) ;
#7803 = DIRECTION ( 'NONE',  ( 0.000000000000000000, 0.000000000000000000, 1.000000000000000000 ) ) ;
#7804 = TOROIDAL_SURFACE ( 'NONE', #1025, 240.0000000000000000, 8.000000000000000000 ) ;
#7805 = AXIS2_PLACEMENT_3D ( 'NONE', #6206, #13027, #3806 ) ;
#7806 = CARTESIAN_POINT ( 'NONE',  ( 25.73052444394193472, 190.4340272497385058, -27.11642929875283059 ) ) ;
#7807 = ADVANCED_FACE ( 'NONE', ( #10881 ), #14872, .T. ) ;
#7808 = DIRECTION ( 'NONE',  ( -1.000000000000000000, -0.000000000000000000, -0.000000000000000000 ) ) ;
#7809 = CIRCLE ( 'NONE', #8667, 2.499999999999998668 ) ;
#7810 = CARTESIAN_POINT ( 'NONE',  ( -12.22383789047832181, 17.99999999999768363, -8.612907111650555336 ) ) ;
#7811 = EDGE_CURVE ( 'NONE', #7814, #2789, #9554, .T. ) ;
#7812 = ADVANCED_FACE ( 'NONE', ( #12394 ), #2835, .T. ) ;
#7813 = VECTOR ( 'NONE', #14070, 1000.000000000000000 ) ;
#7814 = VERTEX_POINT ( 'NONE', #10972 ) ;
#7815 = LINE ( 'NONE', #14462, #5034 ) ;
#7816 = ORIENTED_EDGE ( 'NONE', *, *, #15693, .T. ) ;
#7817 = CARTESIAN_POINT ( 'NONE',  ( 35.61370932537138856, 194.4974200864254783, -26.49149599578360181 ) ) ;
#7818 = DIRECTION ( 'NONE',  ( -1.000000000000000000, 0.000000000000000000, 0.000000000000000000 ) ) ;
#7819 = ORIENTED_EDGE ( 'NONE', *, *, #4273, .T. ) ;
#7820 = ORIENTED_EDGE ( 'NONE', *, *, #15767, .F. ) ;
#7821 = ORIENTED_EDGE ( 'NONE', *, *, #5423, .T. ) ;
#7822 = AXIS2_PLACEMENT_3D ( 'NONE', #9981, #11231, #616 ) ;
#7823 = VECTOR ( 'NONE', #12916, 1000.000000000000000 ) ;
#7824 = CARTESIAN_POINT ( 'NONE',  ( -74.37944869002585335, 151.5947363889490305, -26.22852547856965089 ) ) ;
#7825 = AXIS2_PLACEMENT_3D ( 'NONE', #10850, #5380, #8202 ) ;
#7826 = VERTEX_POINT ( 'NONE', #10719 ) ;
#7827 = CARTESIAN_POINT ( 'NONE',  ( 15.56337975240373162, 125.2134999403455851, -5.000000000000083489 ) ) ;
#7828 = DIRECTION ( 'NONE',  ( -0.000000000000000000, -0.000000000000000000, -1.000000000000000000 ) ) ;
#7829 = CARTESIAN_POINT ( 'NONE',  ( 31.77343803125589616, 152.3723237521624014, -29.23070922465767296 ) ) ;
#7830 = CARTESIAN_POINT ( 'NONE',  ( 21.28500206399612438, 29.87397908709612082, 9.872681979495178339 ) ) ;
#7831 = CARTESIAN_POINT ( 'NONE',  ( 27.99999999999998224, 9.999999999999998224, -16.00000000000000000 ) ) ;
#7832 = ORIENTED_EDGE ( 'NONE', *, *, #8067, .F. ) ;
#7833 = CARTESIAN_POINT ( 'NONE',  ( -40.00000000000000000, 20.00000000000000000, 30.00000000000000355 ) ) ;
#7834 = LINE ( 'NONE', #1019, #16545 ) ;
#7835 = VECTOR ( 'NONE', #13089, 1000.000000000000000 ) ;
#7836 = DIRECTION ( 'NONE',  ( -0.000000000000000000, -0.000000000000000000, -1.000000000000000000 ) ) ;
#7837 = PRODUCT_DEFINITION_FORMATION_WITH_SPECIFIED_SOURCE ( 'ANY', '', #4765, .NOT_KNOWN. ) ;
#7838 = CARTESIAN_POINT ( 'NONE',  ( 15.00000000000000000, 171.6227766016838245, 0.000000000000000000 ) ) ;
#7839 = CARTESIAN_POINT ( 'NONE',  ( 16.24588547270996131, 29.98230316816100327, 14.93526533897157726 ) ) ;
#7840 = ORIENTED_EDGE ( 'NONE', *, *, #991, .T. ) ;
#7841 = LINE ( 'NONE', #13253, #3842 ) ;
#7842 = CARTESIAN_POINT ( 'NONE',  ( -32.99999999999998579, 10.00000000000000000, 28.00000000000000355 ) ) ;
#7843 = EDGE_CURVE ( 'NONE', #9042, #10642, #15690, .T. ) ;
#7844 = ADVANCED_FACE ( 'NONE', ( #16741 ), #1417, .F. ) ;
#7845 = ORIENTED_EDGE ( 'NONE', *, *, #5596, .T. ) ;
#7846 = DIRECTION ( 'NONE',  ( 1.000000000000000000, 0.000000000000000000, 0.000000000000000000 ) ) ;
#7847 = B_SPLINE_CURVE_WITH_KNOTS ( 'NONE', 3,
 ( #1388, #10768, #1118, #14831, #9426, #2711, #6794, #3963, #1293, #9256, #10495, #4050, #12188, #6697, #9077, #15900, #7933, #2439, #14485, #3770, #9164, #11819, #6606, #2352, #12097 ),
 .UNSPECIFIED., .F., .F.,
 ( 4, 2, 2, 1, 2, 2, 2, 2, 2, 2, 2, 2, 4 ),
 ( 0.000000000000000000, 0.003937549356687076833, 0.005906324035030613949, 0.007875098713374151932, 0.009843873391717689048, 0.01181264807006122616, 0.01575019742674830733, 0.01771897210509184445, 0.01968774678343538503, 0.02362529614012245927, 0.02559407081846599985, 0.02756284549680953697, 0.03150039485349661467 ),
 .UNSPECIFIED. ) ;
#7848 = EDGE_LOOP ( 'NONE', ( #1382, #15338 ) ) ;
#7849 = FILL_AREA_STYLE_COLOUR ( '', #8146 ) ;
#7850 = AXIS2_PLACEMENT_3D ( 'NONE', #3410, #12871, #17112 ) ;
#7851 = CARTESIAN_POINT ( 'NONE',  ( -84.18069928808040459, 143.8651737624333862, 17.85267748742823457 ) ) ;
#7852 = CARTESIAN_POINT ( 'NONE',  ( -15.00000000000001421, 130.0000000000000000, -13.00000000000000000 ) ) ;
#7853 = DIRECTION ( 'NONE',  ( 0.000000000000000000, 0.000000000000000000, 1.000000000000000000 ) ) ;
#7854 = DIRECTION ( 'NONE',  ( -1.000000000000000000, 0.000000000000000000, 8.673617379884037937E-17 ) ) ;
#7855 = ORIENTED_EDGE ( 'NONE', *, *, #6657, .F. ) ;
#7856 = CARTESIAN_POINT ( 'NONE',  ( 15.00000000000000000, 143.0344144757318929, 16.50549856913627877 ) ) ;
#7857 = CARTESIAN_POINT ( 'NONE',  ( -208.0711340499744040, 172.7728173183454601, -5.647621413624758446 ) ) ;
#7858 = CARTESIAN_POINT ( 'NONE',  ( -40.00000000000000000, 4.000000000000000000, -30.00000000000000711 ) ) ;
#7859 = PRESENTATION_STYLE_ASSIGNMENT (( #5204 ) ) ;
#7860 = ORIENTED_EDGE ( 'NONE', *, *, #14504, .F. ) ;
#7861 = VECTOR ( 'NONE', #789, 1000.000000000000000 ) ;
#7862 = ORIENTED_EDGE ( 'NONE', *, *, #10597, .T. ) ;
#7863 = CARTESIAN_POINT ( 'NONE',  ( 10.15450428991780285, 132.7081580017661224, -14.27405243007192581 ) ) ;
#7864 = EDGE_CURVE ( 'NONE', #8265, #647, #10428, .T. ) ;
#7865 = EDGE_CURVE ( 'NONE', #489, #4595, #9819, .T. ) ;
#7866 = EDGE_CURVE ( 'NONE', #13670, #12384, #4520, .T. ) ;
#7867 = ORIENTED_EDGE ( 'NONE', *, *, #11333, .T. ) ;
#7868 = CARTESIAN_POINT ( 'NONE',  ( -85.04057431567690628, 149.8830506427268290, -27.43035542581613129 ) ) ;
#7869 = EDGE_CURVE ( 'NONE', #10091, #3188, #3099, .T. ) ;
#7870 = CARTESIAN_POINT ( 'NONE',  ( 19.90854668962690255, 142.0789032940274410, -14.70609183182490298 ) ) ;
#7871 = ORIENTED_EDGE ( 'NONE', *, *, #15095, .T. ) ;
#7872 = CARTESIAN_POINT ( 'NONE',  ( -33.00000000000000711, 171.6227766016838245, -5.000000000000007994 ) ) ;
#7873 = DIRECTION ( 'NONE',  ( 0.000000000000000000, -0.000000000000000000, 1.000000000000000000 ) ) ;
#7874 = CARTESIAN_POINT ( 'NONE',  ( -100.0000000000000000, 171.6227766016838245, -30.00000000000000711 ) ) ;
#7875 = CIRCLE ( 'NONE', #251, 2.500000000000002220 ) ;
#7876 = CONICAL_SURFACE ( 'NONE', #2806, 33.26794919243112503, 0.5235987755983005920 ) ;
#7877 = CARTESIAN_POINT ( 'NONE',  ( 39.99999999999998579, 4.000000000000000000, -33.00000000000000711 ) ) ;
#7878 = CIRCLE ( 'NONE', #14126, 5.000000000000000888 ) ;
#7879 = CARTESIAN_POINT ( 'NONE',  ( -32.99999999999998579, 10.00000000000000000, 35.00200000000000244 ) ) ;
#7880 = CARTESIAN_POINT ( 'NONE',  ( 22.73076297281406255, 29.84603606043824442, -6.815711530131156159 ) ) ;
#7881 = LINE ( 'NONE', #8801, #11762 ) ;
#7882 = DIRECTION ( 'NONE',  ( -0.000000000000000000, -0.000000000000000000, -1.000000000000000000 ) ) ;
#7883 = DIRECTION ( 'NONE',  ( 0.000000000000000000, 0.000000000000000000, 1.000000000000000000 ) ) ;
#7884 = SURFACE_STYLE_USAGE ( .BOTH. , #16216 ) ;
#7885 = EDGE_LOOP ( 'NONE', ( #9051, #7921 ) ) ;
#7886 = CARTESIAN_POINT ( 'NONE',  ( 14.80502546477524817, 129.0472650296936479, -11.28997929065621797 ) ) ;
#7887 = CARTESIAN_POINT ( 'NONE',  ( -23.65835920965562877, 20.00000000000000000, -17.33937328557894020 ) ) ;
#7888 = EDGE_LOOP ( 'NONE', ( #4492, #11707, #12824, #8526 ) ) ;
#7889 = EDGE_CURVE ( 'NONE', #12193, #7826, #16687, .T. ) ;
#7890 = LINE ( 'NONE', #12144, #16678 ) ;
#7891 = AXIS2_PLACEMENT_3D ( 'NONE', #14328, #7680, #11585 ) ;
#7892 = DIRECTION ( 'NONE',  ( 1.000000000000000000, 0.000000000000000000, 0.000000000000000000 ) ) ;
#7893 = AXIS2_PLACEMENT_3D ( 'NONE', #3918, #9303, #17456 ) ;
#7894 = VERTEX_POINT ( 'NONE', #11498 ) ;
#7895 = CARTESIAN_POINT ( 'NONE',  ( 27.50000000000000355, 196.6227766016838245, 10.00000000000000178 ) ) ;
#7896 = AXIS2_PLACEMENT_3D ( 'NONE', #7292, #10116, #15605 ) ;
#7897 = CARTESIAN_POINT ( 'NONE',  ( 20.41303537789175948, 141.9260521957599508, 14.39564681615556907 ) ) ;
#7898 = VERTEX_POINT ( 'NONE', #8672 ) ;
#7899 = CARTESIAN_POINT ( 'NONE',  ( -725.0000000000000000, 19.99999999999995737, -15.00000000000000000 ) ) ;
#7900 = EDGE_LOOP ( 'NONE', ( #4616, #16565 ) ) ;
#7901 = CARTESIAN_POINT ( 'NONE',  ( 16.17028938446068764, 143.0439382767918346, -16.49999999999050360 ) ) ;
#7902 = CARTESIAN_POINT ( 'NONE',  ( 29.69361278289504114, 189.1234298779548624, -27.97726104294733673 ) ) ;
#7903 = CIRCLE ( 'NONE', #3090, 12.00000000000000000 ) ;
#7904 = PLANE ( 'NONE',  #51 ) ;
#7905 = CARTESIAN_POINT ( 'NONE',  ( -11.06002279671335131, 18.00000000000227374, -10.55202560282026703 ) ) ;
#7906 = AXIS2_PLACEMENT_3D ( 'NONE', #1256, #17466, #5337 ) ;
#7907 = VERTEX_POINT ( 'NONE', #16817 ) ;
#7908 = FACE_OUTER_BOUND ( 'NONE', #4725, .T. ) ;
#7909 = ORIENTED_EDGE ( 'NONE', *, *, #2912, .F. ) ;
#7910 = EDGE_CURVE ( 'NONE', #10903, #5469, #2557, .T. ) ;
#7911 = CARTESIAN_POINT ( 'NONE',  ( 36.00000000000002132, 195.9827547425046816, -25.14811700250533733 ) ) ;
#7912 = CARTESIAN_POINT ( 'NONE',  ( -206.3689767832464668, 173.6103877383153247, 4.531616471133065538 ) ) ;
#7913 = ORIENTED_EDGE ( 'NONE', *, *, #5054, .T. ) ;
#7914 = ORIENTED_EDGE ( 'NONE', *, *, #9808, .T. ) ;
#7915 = VERTEX_POINT ( 'NONE', #5125 ) ;
#7916 = VECTOR ( 'NONE', #15221, 1000.000000000000000 ) ;
#7917 = ADVANCED_FACE ( 'NONE', ( #4781 ), #8839, .T. ) ;
#7918 = CARTESIAN_POINT ( 'NONE',  ( 27.99999999999998224, 9.999999999999998224, 28.00000000000001066 ) ) ;
#7919 = AXIS2_PLACEMENT_3D ( 'NONE', #6619, #3976, #5195 ) ;
#7920 = EDGE_CURVE ( 'NONE', #8790, #3840, #15260, .T. ) ;
#7921 = ORIENTED_EDGE ( 'NONE', *, *, #15361, .F. ) ;
#7922 = CARTESIAN_POINT ( 'NONE',  ( 27.48361012698968864, 138.6227766016838245, -1.063447695028167043E-14 ) ) ;
#7923 = CARTESIAN_POINT ( 'NONE',  ( 22.99999999999997868, 9.999999999999998224, 0.000000000000000000 ) ) ;
#7924 = SHAPE_REPRESENTATION ( 'MirrorLeft Housing Shell', ( #3583 ), #11532 ) ;
#7925 = DIRECTION ( 'NONE',  ( -1.000000000000000000, 0.000000000000000000, 0.000000000000000000 ) ) ;
#7926 = DIRECTION ( 'NONE',  ( -1.000000000000000000, -0.000000000000000000, -0.000000000000000000 ) ) ;
#7927 = CYLINDRICAL_SURFACE ( 'NONE', #4373, 2.500000000000000444 ) ;
#7928 = ORIENTED_EDGE ( 'NONE', *, *, #13498, .F. ) ;
#7929 = CARTESIAN_POINT ( 'NONE',  ( -80.90809021110644039, 202.5550951275239413, -16.37659873159346446 ) ) ;
#7930 = VECTOR ( 'NONE', #15717, 1000.000000000000000 ) ;
#7931 = CARTESIAN_POINT ( 'NONE',  ( 24.60077399342406679, 29.87270634359742871, -7.584611049657961068 ) ) ;
#7932 = CARTESIAN_POINT ( 'NONE',  ( 11.67974368446408384, 131.7296502858855547, 13.62018484423547804 ) ) ;
#7933 = CARTESIAN_POINT ( 'NONE',  ( 32.29638371061065527, 18.00000000000000000, 15.01265034258821096 ) ) ;
#7934 = AXIS2_PLACEMENT_3D ( 'NONE', #4751, #596, #13964 ) ;
#7935 = CARTESIAN_POINT ( 'NONE',  ( 14.93242934743711992, 30.00000000000000000, 15.00000000000000000 ) ) ;
#7936 = VERTEX_POINT ( 'NONE', #8919 ) ;
#7937 = FACE_OUTER_BOUND ( 'NONE', #1892, .T. ) ;
#7938 = PRODUCT_RELATED_PRODUCT_CATEGORY ( 'part', '', ( #8417 ) ) ;
#7939 = DIRECTION ( 'NONE',  ( -1.000000000000000000, 0.000000000000000000, 0.000000000000000000 ) ) ;
#7940 = ORIENTED_EDGE ( 'NONE', *, *, #13564, .F. ) ;
#7941 = PRESENTATION_STYLE_ASSIGNMENT (( #11654 ) ) ;
#7942 = DIRECTION ( 'NONE',  ( -1.000000000000000000, 0.000000000000000000, 0.000000000000000000 ) ) ;
#7943 = EDGE_CURVE ( 'NONE', #15082, #7515, #15574, .T. ) ;
#7944 = AXIS2_PLACEMENT_3D ( 'NONE', #1470, #4044, #9506 ) ;
#7945 = VERTEX_POINT ( 'NONE', #13009 ) ;
#7946 = CARTESIAN_POINT ( 'NONE',  ( -80.24502126479927711, 141.6230733471410304, 13.74837463607935284 ) ) ;
#7947 = CARTESIAN_POINT ( 'NONE',  ( 14.93242934743710570, 18.00000000000000355, -12.99999999999999822 ) ) ;
#7948 = CARTESIAN_POINT ( 'NONE',  ( -75.67138096537212277, 142.4529008285661575, -19.34799176589369196 ) ) ;
#7949 = CARTESIAN_POINT ( 'NONE',  ( -23.65835920965562877, 20.00000000000000000, 17.33937328557894020 ) ) ;
#7950 = ORIENTED_EDGE ( 'NONE', *, *, #8067, .T. ) ;
#7951 = CARTESIAN_POINT ( 'NONE',  ( -103.0000000000000142, 171.6227766016838245, 6.000000000000005329 ) ) ;
#7952 = CARTESIAN_POINT ( 'NONE',  ( -33.00000000000000711, 171.6227766016838245, -5.000000000000007994 ) ) ;
#7953 = EDGE_CURVE ( 'NONE', #10603, #1036, #9011, .T. ) ;
#7954 = DIRECTION ( 'NONE',  ( 0.1091791256177803426, -0.4970110457850390184, 0.8608483832226199173 ) ) ;
#7955 = FACE_OUTER_BOUND ( 'NONE', #8436, .T. ) ;
#7956 = VECTOR ( 'NONE', #4024, 1000.000000000000000 ) ;
#7957 = ORIENTED_EDGE ( 'NONE', *, *, #10861, .T. ) ;
#7958 = CARTESIAN_POINT ( 'NONE',  ( 9.474973892937489595, 133.0798911729450538, -14.49933486760529355 ) ) ;
#7959 = VERTEX_POINT ( 'NONE', #17071 ) ;
#7960 = CARTESIAN_POINT ( 'NONE',  ( -82.42159468966464431, 152.1166601635960376, -29.06070213693889670 ) ) ;
#7961 = CARTESIAN_POINT ( 'NONE',  ( 14.40670567839409344, 127.3124839991112083, -8.619616438334361419 ) ) ;
#7962 = ORIENTED_EDGE ( 'NONE', *, *, #2836, .T. ) ;
#7963 = DIRECTION ( 'NONE',  ( -0.000000000000000000, -0.000000000000000000, -1.000000000000000000 ) ) ;
#7964 = CARTESIAN_POINT ( 'NONE',  ( -43.00000000000003553, 134.2062027339443944, 13.00000000000000000 ) ) ;
#7965 = DIRECTION ( 'NONE',  ( -1.000000000000000000, -0.000000000000000000, 0.000000000000000000 ) ) ;
#7966 = DIRECTION ( 'NONE',  ( -0.000000000000000000, -0.000000000000000000, -1.000000000000000000 ) ) ;
#7967 = DIRECTION ( 'NONE',  ( 1.000000000000000000, 0.000000000000000000, 0.000000000000000000 ) ) ;
#7968 = CARTESIAN_POINT ( 'NONE',  ( 21.28500206399612438, 29.87397908709612082, -9.872681979495178339 ) ) ;
#7969 = LINE ( 'NONE', #3810, #472 ) ;
#7970 = CARTESIAN_POINT ( 'NONE',  ( 196.0000000000000000, 167.6227766016838530, -8.071800142134975431 ) ) ;
#7971 = ADVANCED_FACE ( 'NONE', ( #9184 ), #10515, .F. ) ;
#7972 = EDGE_CURVE ( 'NONE', #5354, #4853, #9889, .T. ) ;
#7973 = CARTESIAN_POINT ( 'NONE',  ( -725.0000000000000000, 130.0000000000000000, -13.00000000000000000 ) ) ;
#7974 = EDGE_CURVE ( 'NONE', #16285, #10197, #16963, .T. ) ;
#7975 = CARTESIAN_POINT ( 'NONE',  ( 25.21634339652309365, 142.9837419059134334, -20.12545249291982330 ) ) ;
#7976 = ORIENTED_EDGE ( 'NONE', *, *, #2055, .F. ) ;
#7977 = DIRECTION ( 'NONE',  ( -0.000000000000000000, -0.000000000000000000, -1.000000000000000000 ) ) ;
#7978 = VERTEX_POINT ( 'NONE', #3621 ) ;
#7979 = CARTESIAN_POINT ( 'NONE',  ( -23.00000000000000000, 120.0000000000000284, 4.999999999999999112 ) ) ;
#7980 = DIRECTION ( 'NONE',  ( -1.000000000000000000, 0.000000000000000000, 0.000000000000000000 ) ) ;
#7981 = VERTEX_POINT ( 'NONE', #15918 ) ;
#7982 = CARTESIAN_POINT ( 'NONE',  ( -9.825395436088792067, 30.54854208321445341, 14.75250191942001088 ) ) ;
#7983 = CARTESIAN_POINT ( 'NONE',  ( 13.73607130285257227, 138.7967234794239459, 3.453855393586055200 ) ) ;
#7984 = ORIENTED_EDGE ( 'NONE', *, *, #2896, .F. ) ;
#7985 = FACE_OUTER_BOUND ( 'NONE', #8661, .T. ) ;
#7986 = EDGE_LOOP ( 'NONE', ( #11977, #9195, #3448, #2688, #16696, #5042 ) ) ;
#7987 = CARTESIAN_POINT ( 'NONE',  ( 27.50000000000000355, 196.6227766016838245, 1.387778780781445676E-14 ) ) ;
#7988 = CARTESIAN_POINT ( 'NONE',  ( 48.00000000000000711, 187.6227766016837961, 10.00000337241049309 ) ) ;
#7989 = CYLINDRICAL_SURFACE ( 'NONE', #3435, 5.000000000000000888 ) ;
#7990 = CARTESIAN_POINT ( 'NONE',  ( -12.66151707385411740, 17.99999999999770495, -6.998435355972849159 ) ) ;
#7991 = ORIENTED_EDGE ( 'NONE', *, *, #4685, .T. ) ;
#7992 = CARTESIAN_POINT ( 'NONE',  ( 26.57851455615899994, 150.2853719096988812, 25.17531865327014629 ) ) ;
#7993 = ORIENTED_EDGE ( 'NONE', *, *, #1465, .T. ) ;
#7994 = CARTESIAN_POINT ( 'NONE',  ( -73.02032457293853440, 193.8447098639589683, -24.40281628369250555 ) ) ;
#7995 = DIRECTION ( 'NONE',  ( -0.08715574274765379437, 0.9961946980917459893, 0.000000000000000000 ) ) ;
#7996 = ORIENTED_EDGE ( 'NONE', *, *, #13635, .T. ) ;
#7997 = ORIENTED_EDGE ( 'NONE', *, *, #1438, .F. ) ;
#7998 = ORIENTED_EDGE ( 'NONE', *, *, #1101, .T. ) ;
#7999 = DIRECTION ( 'NONE',  ( 0.000000000000000000, 0.000000000000000000, 1.000000000000000000 ) ) ;
#8000 = ORIENTED_EDGE ( 'NONE', *, *, #3705, .T. ) ;
#8001 = APPLICATION_PROTOCOL_DEFINITION ( 'draft international standard', 'automotive_design', 1998, #10711 ) ;
#8002 = CARTESIAN_POINT ( 'NONE',  ( -20.00000000000000355, 171.6227766016838245, 0.000000000000000000 ) ) ;
#8003 = EDGE_CURVE ( 'NONE', #17055, #3234, #5944, .T. ) ;
#8004 = CARTESIAN_POINT ( 'NONE',  ( -16.66926302330761800, 31.99181794709938487, 10.22419352058821396 ) ) ;
#8005 = CARTESIAN_POINT ( 'NONE',  ( 24.95942568432312214, 149.8830506427267721, -27.43035542581612773 ) ) ;
#8006 = CARTESIAN_POINT ( 'NONE',  ( -90.80384757729339640, 204.6227766016838245, 0.000000000000000000 ) ) ;
#8007 = CARTESIAN_POINT ( 'NONE',  ( -80.99255306636646878, 151.5270838226223873, 26.17568438743892045 ) ) ;
#8008 = ORIENTED_EDGE ( 'NONE', *, *, #10013, .T. ) ;
#8009 = DIRECTION ( 'NONE',  ( 0.000000000000000000, 1.000000000000000000, 0.000000000000000000 ) ) ;
#8010 = DIRECTION ( 'NONE',  ( 0.000000000000000000, 0.000000000000000000, 1.000000000000000000 ) ) ;
#8011 = CARTESIAN_POINT ( 'NONE',  ( 196.0000000000000000, 183.6227766016837961, 3.071800142134975431 ) ) ;
#8012 = CARTESIAN_POINT ( 'NONE',  ( 48.00000000000000711, 171.6227766016838245, 0.000000000000000000 ) ) ;
#8013 = CARTESIAN_POINT ( 'NONE',  ( -48.00000000000000000, 171.6227766016838245, 20.00000000000000355 ) ) ;
#8014 = EDGE_LOOP ( 'NONE', ( #10910, #17360, #17038, #1982 ) ) ;
#8015 = DIRECTION ( 'NONE',  ( -1.000000000000000000, 0.000000000000000000, -0.000000000000000000 ) ) ;
#8016 = LINE ( 'NONE', #1630, #8039 ) ;
#8017 = CARTESIAN_POINT ( 'NONE',  ( 32.50000000000000711, 146.6227766016838245, 10.00000000000000178 ) ) ;
#8018 = VERTEX_POINT ( 'NONE', #6446 ) ;
#8019 = CARTESIAN_POINT ( 'NONE',  ( -80.00000000000002842, 146.6227766016838245, -16.00000000000000000 ) ) ;
#8020 = EDGE_LOOP ( 'NONE', ( #8586, #7673 ) ) ;
#8021 = CARTESIAN_POINT ( 'NONE',  ( -75.13467353717234687, 145.4324535730256969, 20.08206597984644048 ) ) ;
#8022 = EDGE_CURVE ( 'NONE', #11848, #9167, #8478, .T. ) ;
#8023 = CARTESIAN_POINT ( 'NONE',  ( -27.99999999999998224, 10.00000000000000000, -28.00000000000000355 ) ) ;
#8024 = AXIS2_PLACEMENT_3D ( 'NONE', #10073, #5669, #9904 ) ;
#8025 = CARTESIAN_POINT ( 'NONE',  ( -77.58995968165618251, 141.1235162643940839, -17.17043012754695397 ) ) ;
#8026 = CARTESIAN_POINT ( 'NONE',  ( -34.99999999999999289, 122.0000000000000000, 0.000000000000000000 ) ) ;
#8027 = VERTEX_POINT ( 'NONE', #956 ) ;
#8028 = DIRECTION ( 'NONE',  ( -1.000000000000000000, 0.000000000000000000, -2.312964634635742464E-16 ) ) ;
#8029 = ADVANCED_FACE ( 'NONE', ( #2109 ), #796, .F. ) ;
#8030 = LINE ( 'NONE', #14683, #13563 ) ;
#8031 = DIRECTION ( 'NONE',  ( -1.000000000000000000, 0.000000000000000000, 0.000000000000000000 ) ) ;
#8032 = ADVANCED_FACE ( 'NONE', ( #10424, #6543 ), #2467, .T. ) ;
#8033 = CARTESIAN_POINT ( 'NONE',  ( -33.99999999999997868, 10.00000000000000000, -30.00000000000000355 ) ) ;
#8034 = EDGE_CURVE ( 'NONE', #11303, #14615, #14150, .T. ) ;
#8035 = ORIENTED_EDGE ( 'NONE', *, *, #5983, .T. ) ;
#8036 = ADVANCED_BREP_SHAPE_REPRESENTATION ( '', ( #17066, #3583 ), #11532 ) ;
#8037 = AXIS2_PLACEMENT_3D ( 'NONE', #10740, #9575, #14981 ) ;
#8038 = CARTESIAN_POINT ( 'NONE',  ( 14.92319712166297840, 137.6313713749889587, -10.11910373048704770 ) ) ;
#8039 = VECTOR ( 'NONE', #4464, 1000.000000000000000 ) ;
#8040 = ORIENTED_EDGE ( 'NONE', *, *, #13824, .F. ) ;
#8041 = CARTESIAN_POINT ( 'NONE',  ( -79.55900457720692032, 152.6108673192418337, -29.38619085311482948 ) ) ;
#8042 = CARTESIAN_POINT ( 'NONE',  ( 12.08578903453337183, 130.1663611114758510, -11.02150463548631976 ) ) ;
#8043 = ORIENTED_EDGE ( 'NONE', *, *, #2843, .F. ) ;
#8044 = EDGE_CURVE ( 'NONE', #134, #17383, #287, .T. ) ;
#8045 = DIRECTION ( 'NONE',  ( -1.000000000000000000, -0.000000000000000000, 0.000000000000000000 ) ) ;
#8046 = CARTESIAN_POINT ( 'NONE',  ( -138.7106781186547266, 171.6227766016838245, 24.99999999999999289 ) ) ;
#8047 = DIRECTION ( 'NONE',  ( -1.000000000000000000, 0.000000000000000000, 0.000000000000000000 ) ) ;
#8048 = DIRECTION ( 'NONE',  ( -1.000000000000000000, -0.000000000000000000, -0.000000000000000000 ) ) ;
#8049 = CARTESIAN_POINT ( 'NONE',  ( 23.79315516583586643, 18.00000000000000000, -22.94240041036162836 ) ) ;
#8050 = AXIS2_PLACEMENT_3D ( 'NONE', #13028, #11677, #3465 ) ;
#8051 = CARTESIAN_POINT ( 'NONE',  ( 20.95008785553089581, 29.88049067427350280, -10.28044474760307914 ) ) ;
#8052 = CARTESIAN_POINT ( 'NONE',  ( 2.750000000000000000, 3.306546357697852747E-16, -2.699999999999999289 ) ) ;
#8053 = LINE ( 'NONE', #13463, #6478 ) ;
#8054 = DIRECTION ( 'NONE',  ( -1.000000000000000000, 0.000000000000000000, 0.000000000000000000 ) ) ;
#8055 = EDGE_LOOP ( 'NONE', ( #12067, #10565, #16870, #15840 ) ) ;
#8056 = DIRECTION ( 'NONE',  ( -0.08715574274765344742, -0.4980973490458779906, 0.8627299156628184251 ) ) ;
#8057 = ORIENTED_EDGE ( 'NONE', *, *, #16700, .T. ) ;
#8058 = FACE_BOUND ( 'NONE', #7724, .T. ) ;
#8059 = CARTESIAN_POINT ( 'NONE',  ( -8.719536044788691598, 18.00000000000000711, -25.00000000000000000 ) ) ;
#8060 = VERTEX_POINT ( 'NONE', #10171 ) ;
#8061 = CARTESIAN_POINT ( 'NONE',  ( -12.16365208422963740, 31.05675767351161909, 14.01395464075509878 ) ) ;
#8062 = CARTESIAN_POINT ( 'NONE',  ( 27.44407568426053246, 138.8271129316868837, 3.666666666666671404 ) ) ;
#8063 = EDGE_CURVE ( 'NONE', #2973, #4989, #17250, .T. ) ;
#8064 = ORIENTED_EDGE ( 'NONE', *, *, #5830, .F. ) ;
#8065 = ADVANCED_FACE ( 'NONE', ( #13270 ), #10252, .T. ) ;
#8066 = DIRECTION ( 'NONE',  ( 1.000000000000000000, 0.000000000000000000, -0.000000000000000000 ) ) ;
#8067 = EDGE_CURVE ( 'NONE', #16869, #9322, #6797, .T. ) ;
#8068 = AXIS2_PLACEMENT_3D ( 'NONE', #6324, #11719, #17129 ) ;
#8069 = ORIENTED_EDGE ( 'NONE', *, *, #7430, .F. ) ;
#8070 = DIRECTION ( 'NONE',  ( 1.000000000000000000, -0.000000000000000000, -0.000000000000000000 ) ) ;
#8071 = CARTESIAN_POINT ( 'NONE',  ( 37.50000000000000711, 196.6227766016838245, -21.54065922853802562 ) ) ;
#8072 = DIRECTION ( 'NONE',  ( -1.156482317317868274E-16, 1.000000000000000000, 0.000000000000000000 ) ) ;
#8073 = CARTESIAN_POINT ( 'NONE',  ( 32.99999999999998579, 9.999999999999998224, 0.000000000000000000 ) ) ;
#8074 = ORIENTED_EDGE ( 'NONE', *, *, #15767, .T. ) ;
#8075 = CARTESIAN_POINT ( 'NONE',  ( 49.99999999999998579, 167.6227766016838814, -16.92820660268601429 ) ) ;
#8076 = VECTOR ( 'NONE', #11025, 1000.000000000000000 ) ;
#8077 = VERTEX_POINT ( 'NONE', #10598 ) ;
#8078 = CARTESIAN_POINT ( 'NONE',  ( -208.1243153690002714, 176.1535417859606980, -3.744436563795452866 ) ) ;
#8079 = CARTESIAN_POINT ( 'NONE',  ( -14.99999999999999467, 90.00000000000000000, -15.00000000000000000 ) ) ;
#8080 = ORIENTED_EDGE ( 'NONE', *, *, #14108, .T. ) ;
#8081 = AXIS2_PLACEMENT_3D ( 'NONE', #6981, #9450, #15030 ) ;
#8082 = EDGE_LOOP ( 'NONE', ( #2052, #15584, #9849, #5605 ) ) ;
#8083 = ORIENTED_EDGE ( 'NONE', *, *, #790, .F. ) ;
#8084 = EDGE_CURVE ( 'NONE', #9221, #5721, #5660, .T. ) ;
#8085 = EDGE_CURVE ( 'NONE', #11298, #15769, #5202, .T. ) ;
#8086 = CYLINDRICAL_SURFACE ( 'NONE', #3343, 5.000000000000018652 ) ;
#8087 = AXIS2_PLACEMENT_3D ( 'NONE', #5856, #366, #11156 ) ;
#8088 = ORIENTED_EDGE ( 'NONE', *, *, #14110, .T. ) ;
#8089 = CARTESIAN_POINT ( 'NONE',  ( -80.00000000000002842, 146.6227766016838245, 0.000000000000000000 ) ) ;
#8090 = AXIS2_PLACEMENT_3D ( 'NONE', #11704, #13133, #1002 ) ;
#8091 = CARTESIAN_POINT ( 'NONE',  ( -95.00000000000000000, 141.6227766016838245, -5.510910596163088767E-15 ) ) ;
#8092 = CARTESIAN_POINT ( 'NONE',  ( 20.96141083122825322, 29.88026331201747254, -10.28670731940101923 ) ) ;
#8093 = CARTESIAN_POINT ( 'NONE',  ( 15.00000000000000000, 171.6227766016838245, 0.000000000000000000 ) ) ;
#8094 = CARTESIAN_POINT ( 'NONE',  ( -75.34926945688242483, 148.4807726931354068, 23.52860204907123887 ) ) ;
#8095 = VERTEX_POINT ( 'NONE', #9442 ) ;
#8096 = CARTESIAN_POINT ( 'NONE',  ( -85.99137549878169295, 196.9927911392394151, -24.11293157882131766 ) ) ;
#8097 = DIRECTION ( 'NONE',  ( 0.000000000000000000, 0.000000000000000000, -1.000000000000000000 ) ) ;
#8098 = CARTESIAN_POINT ( 'NONE',  ( 39.99999999999998579, 8.000000000000000000, -29.99999999999999645 ) ) ;
#8099 = CARTESIAN_POINT ( 'NONE',  ( -206.3689767832464668, 173.6103877383153247, 4.531616471133065538 ) ) ;
#8100 = DIRECTION ( 'NONE',  ( 1.000000000000000000, 0.000000000000000000, 0.000000000000000000 ) ) ;
#8101 = CIRCLE ( 'NONE', #6969, 28.26633746182136164 ) ;
#8102 = CIRCLE ( 'NONE', #121, 1.500000000000000000 ) ;
#8103 = AXIS2_PLACEMENT_3D ( 'NONE', #8227, #8399, #4428 ) ;
#8104 = EDGE_CURVE ( 'NONE', #10900, #6066, #14978, .T. ) ;
#8105 = MECHANICAL_DESIGN_GEOMETRIC_PRESENTATION_REPRESENTATION (  '', ( #13501 ), #7263 ) ;
#8106 = AXIS2_PLACEMENT_3D ( 'NONE', #806, #4614, #8769 ) ;
#8107 = DIRECTION ( 'NONE',  ( 1.000000000000000000, 0.000000000000000000, 0.000000000000000000 ) ) ;
#8108 = VERTEX_POINT ( 'NONE', #14074 ) ;
#8109 = DIRECTION ( 'NONE',  ( 0.000000000000000000, 0.000000000000000000, -1.000000000000000000 ) ) ;
#8110 = ORIENTED_EDGE ( 'NONE', *, *, #6233, .F. ) ;
#8111 = DIRECTION ( 'NONE',  ( 1.000000000000000000, 0.000000000000000000, -0.000000000000000000 ) ) ;
#8112 = DIRECTION ( 'NONE',  ( -1.000000000000000000, -0.000000000000000000, -0.000000000000000000 ) ) ;
#8113 = CARTESIAN_POINT ( 'NONE',  ( -207.8780901672884056, 166.2720010150300425, 1.419081159745146259 ) ) ;
#8114 = VECTOR ( 'NONE', #11496, 1000.000000000000000 ) ;
#8115 = MECHANICAL_DESIGN_GEOMETRIC_PRESENTATION_REPRESENTATION (  '', ( #9239 ), #16325 ) ;
#8116 = CARTESIAN_POINT ( 'NONE',  ( 24.93507336697352628, 29.86842105263157876, 4.999999999999999112 ) ) ;
#8117 =( GEOMETRIC_REPRESENTATION_CONTEXT ( 3 ) GLOBAL_UNCERTAINTY_ASSIGNED_CONTEXT ( ( #5086 ) ) GLOBAL_UNIT_ASSIGNED_CONTEXT ( ( #16360, #2972, #13614 ) ) REPRESENTATION_CONTEXT ( 'NONE', 'WORKASPACE' ) );
#8118 = ORIENTED_EDGE ( 'NONE', *, *, #15385, .T. ) ;
#8119 = CARTESIAN_POINT ( 'NONE',  ( 196.0000000000000000, 171.6227766016838245, -12.50000337241049131 ) ) ;
#8120 = CARTESIAN_POINT ( 'NONE',  ( -24.93725393319378725, 100.0000000000000142, 5.500000000000000000 ) ) ;
#8121 = DIRECTION ( 'NONE',  ( 0.000000000000000000, -1.000000000000000000, -8.673617379884037444E-16 ) ) ;
#8122 = CARTESIAN_POINT ( 'NONE',  ( 35.34723643798712800, 199.3666727680386828, -21.34312735376096626 ) ) ;
#8123 = PRODUCT_DEFINITION_SHAPE ( 'NONE', 'NONE',  #17528 ) ;
#8124 = EDGE_CURVE ( 'NONE', #12106, #11342, #12206, .T. ) ;
#8125 =( BOUNDED_CURVE ( )  B_SPLINE_CURVE ( 3, ( #7743, #13152, #16979, #7411 ),
 .UNSPECIFIED., .F., .F. ) 
 B_SPLINE_CURVE_WITH_KNOTS ( ( 4, 4 ),
 ( 1.570796326794899000, 3.141592653589791340 ),
 .UNSPECIFIED. ) 
 CURVE ( )  GEOMETRIC_REPRESENTATION_ITEM ( )  RATIONAL_B_SPLINE_CURVE ( ( 1.000000000000000000, 0.8047378541243659367, 0.8047378541243659367, 1.000000000000000000 ) ) 
 REPRESENTATION_ITEM ( '' )  );
#8126 = FACE_OUTER_BOUND ( 'NONE', #7900, .T. ) ;
#8127 = AXIS2_PLACEMENT_3D ( 'NONE', #2369, #14423, #8915 ) ;
#8128 = ORIENTED_EDGE ( 'NONE', *, *, #446, .T. ) ;
#8129 = PRODUCT_DEFINITION_FORMATION_WITH_SPECIFIED_SOURCE ( 'ANY', '', #1782, .NOT_KNOWN. ) ;
#8130 = CARTESIAN_POINT ( 'NONE',  ( -74.44332442587726462, 148.9132954376224518, -26.63594553516328034 ) ) ;
#8131 = AXIS2_PLACEMENT_3D ( 'NONE', #5992, #8730, #16621 ) ;
#8132 = CARTESIAN_POINT ( 'NONE',  ( -208.0000000000000853, 174.7326106162513497, 0.000000000000000000 ) ) ;
#8133 = ORIENTED_EDGE ( 'NONE', *, *, #15224, .F. ) ;
#8134 = CARTESIAN_POINT ( 'NONE',  ( -75.68538708090720490, 192.4344680579923761, -28.14280641908791836 ) ) ;
#8135 = EDGE_CURVE ( 'NONE', #118, #7137, #17425, .T. ) ;
#8136 = ADVANCED_FACE ( 'NONE', ( #1492 ), #4149, .F. ) ;
#8137 = CYLINDRICAL_SURFACE ( 'NONE', #7573, 2.500000000000000444 ) ;
#8138 = CARTESIAN_POINT ( 'NONE',  ( 34.65161675558235999, 194.7673412502506665, 23.52603474534220140 ) ) ;
#8139 = DIRECTION ( 'NONE',  ( 0.000000000000000000, 0.000000000000000000, 1.000000000000000000 ) ) ;
#8140 = CARTESIAN_POINT ( 'NONE',  ( 18.50138388889793362, 17.99999999999999289, -12.24385303908842637 ) ) ;
#8141 = CARTESIAN_POINT ( 'NONE',  ( 39.99999999999998579, 20.00000000000000000, -30.00000000000001066 ) ) ;
#8142 = CYLINDRICAL_SURFACE ( 'NONE', #14953, 6.000000000000005329 ) ;
#8143 = AXIS2_PLACEMENT_3D ( 'NONE', #4047, #13605, #6694 ) ;
#8144 = CARTESIAN_POINT ( 'NONE',  ( 35.00000000000000711, 146.6227766016838245, -35.00200000000000244 ) ) ;
#8145 = AXIS2_PLACEMENT_3D ( 'NONE', #6895, #12292, #15116 ) ;
#8146 = COLOUR_RGB ( '', 0.40784314, 0.44705882, 0.49803922) ;
#8147 = CARTESIAN_POINT ( 'NONE',  ( 25.93662097725987437, 142.1921853732338548, -18.94830881272694612 ) ) ;
#8148 = ORIENTED_EDGE ( 'NONE', *, *, #2349, .T. ) ;
#8149 = CARTESIAN_POINT ( 'NONE',  ( -32.66708739526796279, 101.0000000000000142, 5.500000000000000000 ) ) ;
#8150 = ORIENTED_EDGE ( 'NONE', *, *, #15327, .F. ) ;
#8151 = CARTESIAN_POINT ( 'NONE',  ( 48.00000000000000711, 167.6227766016838530, -3.071800142134975431 ) ) ;
#8152 = DIRECTION ( 'NONE',  ( 1.000000000000000000, 0.000000000000000000, 0.000000000000000000 ) ) ;
#8153 = ORIENTED_EDGE ( 'NONE', *, *, #2452, .T. ) ;
#8154 = CARTESIAN_POINT ( 'NONE',  ( -18.25212770525392614, 32.30769230766699707, 5.660855707253096725 ) ) ;
#8155 = DIRECTION ( 'NONE',  ( 0.000000000000000000, 0.000000000000000000, 1.000000000000000000 ) ) ;
#8156 = ORIENTED_EDGE ( 'NONE', *, *, #10406, .F. ) ;
#8157 = AXIS2_PLACEMENT_3D ( 'NONE', #15149, #5608, #9664 ) ;
#8158 = DIRECTION ( 'NONE',  ( 0.000000000000000000, 0.000000000000000000, -1.000000000000000000 ) ) ;
#8159 = AXIS2_PLACEMENT_3D ( 'NONE', #8666, #11402, #11489 ) ;
#8160 = ORIENTED_EDGE ( 'NONE', *, *, #174, .F. ) ;
#8161 = PLANE ( 'NONE',  #10345 ) ;
#8162 = DIRECTION ( 'NONE',  ( 0.000000000000000000, 0.000000000000000000, -1.000000000000000000 ) ) ;
#8163 = CARTESIAN_POINT ( 'NONE',  ( 196.0000000000000000, 155.6227766016839098, -15.00000337241049486 ) ) ;
#8164 = DIRECTION ( 'NONE',  ( -0.000000000000000000, -1.000000000000000000, -0.000000000000000000 ) ) ;
#8165 = ORIENTED_EDGE ( 'NONE', *, *, #14180, .F. ) ;
#8166 = CARTESIAN_POINT ( 'NONE',  ( -32.93725393319379435, 120.0000000000000284, 5.500000000000000000 ) ) ;
#8167 = AXIS2_PLACEMENT_3D ( 'NONE', #3811, #6562, #10877 ) ;
#8168 = EDGE_CURVE ( 'NONE', #7472, #2271, #11579, .T. ) ;
#8169 = VECTOR ( 'NONE', #7280, 1000.000000000000114 ) ;
#8170 = VERTEX_POINT ( 'NONE', #13443 ) ;
#8171 = CARTESIAN_POINT ( 'NONE',  ( -74.91549491446249931, 191.0841166510127778, -26.65369102675423463 ) ) ;
#8172 = AXIS2_PLACEMENT_3D ( 'NONE', #12808, #16880, #11301 ) ;
#8173 = DIRECTION ( 'NONE',  ( 1.000000000000000000, 0.000000000000000000, 0.000000000000000000 ) ) ;
#8174 = CARTESIAN_POINT ( 'NONE',  ( -32.66708739526796279, 119.0000000000141824, -4.722170599054655860 ) ) ;
#8175 = ORIENTED_EDGE ( 'NONE', *, *, #7524, .F. ) ;
#8176 = ORIENTED_EDGE ( 'NONE', *, *, #2303, .F. ) ;
#8177 = CARTESIAN_POINT ( 'NONE',  ( 7.098239199201186622, 139.5131674267937569, 14.94273745766416184 ) ) ;
#8178 = AXIS2_PLACEMENT_3D ( 'NONE', #16977, #16722, #16884 ) ;
#8179 = ORIENTED_EDGE ( 'NONE', *, *, #13973, .T. ) ;
#8180 = APPLICATION_PROTOCOL_DEFINITION ( 'draft international standard', 'automotive_design', 1998, #2580 ) ;
#8181 = CIRCLE ( 'NONE', #14968, 5.000000000000004441 ) ;
#8182 = DIRECTION ( 'NONE',  ( 0.000000000000000000, 1.000000000000000000, 0.000000000000000000 ) ) ;
#8183 = VECTOR ( 'NONE', #8263, 1000.000000000000000 ) ;
#8184 = FACE_OUTER_BOUND ( 'NONE', #14980, .T. ) ;
#8185 = CARTESIAN_POINT ( 'NONE',  ( 15.00000000000903455, 143.2885527162398489, -16.91661185963483760 ) ) ;
#8186 = CARTESIAN_POINT ( 'NONE',  ( 125.0000000000000000, 0.000000000000000000, 0.000000000000000000 ) ) ;
#8187 = EDGE_LOOP ( 'NONE', ( #10679, #4012 ) ) ;
#8188 = CARTESIAN_POINT ( 'NONE',  ( -81.75466519885634398, 202.3655582339691250, -16.73015311598867783 ) ) ;
#8189 = EDGE_CURVE ( 'NONE', #10010, #2606, #10738, .T. ) ;
#8190 = EDGE_CURVE ( 'NONE', #3129, #713, #1434, .T. ) ;
#8191 = DIRECTION ( 'NONE',  ( -1.000000000000000000, 0.000000000000000000, 0.000000000000000000 ) ) ;
#8192 = ADVANCED_FACE ( 'NONE', ( #5472 ), #2733, .T. ) ;
#8193 = CARTESIAN_POINT ( 'NONE',  ( 33.88556156013721932, 19.99999999999999645, -11.42442012027869858 ) ) ;
#8194 = CARTESIAN_POINT ( 'NONE',  ( -208.0706889292728761, 172.7738155144439531, 5.646695128860279134 ) ) ;
#8195 = DIRECTION ( 'NONE',  ( 0.000000000000000000, 0.000000000000000000, 1.000000000000000000 ) ) ;
#8196 = CIRCLE ( 'NONE', #3978, 3.999999999999998668 ) ;
#8197 = VECTOR ( 'NONE', #1223, 1000.000000000000000 ) ;
#8198 = VERTEX_POINT ( 'NONE', #14849 ) ;
#8199 = TOROIDAL_SURFACE ( 'NONE', #16690, 23.57392898041431195, 2.000000000000000000 ) ;
#8200 = DIRECTION ( 'NONE',  ( 0.000000000000000000, 1.000000000000000000, 0.000000000000000000 ) ) ;
#8201 = EDGE_LOOP ( 'NONE', ( #6384, #670, #2827, #14075, #17040 ) ) ;
#8202 = DIRECTION ( 'NONE',  ( -1.000000000000000000, 0.000000000000000000, 0.000000000000000000 ) ) ;
#8203 = EDGE_LOOP ( 'NONE', ( #11353, #837, #4036, #13276 ) ) ;
#8204 = APPLICATION_PROTOCOL_DEFINITION ( 'draft international standard', 'automotive_design', 1998, #13664 ) ;
#8205 = CARTESIAN_POINT ( 'NONE',  ( 17.58250999372313927, 125.2198453307267414, -1.671679122699602171 ) ) ;
#8206 = DIRECTION ( 'NONE',  ( -0.000000000000000000, 0.000000000000000000, -1.000000000000000000 ) ) ;
#8207 = VECTOR ( 'NONE', #440, 1000.000000000000000 ) ;
#8208 = CARTESIAN_POINT ( 'NONE',  ( -27.98221281347032274, 30.00000000000000000, -4.999999999999996447 ) ) ;
#8209 = VECTOR ( 'NONE', #1020, 1000.000000000000000 ) ;
#8210 = VECTOR ( 'NONE', #12887, 1000.000000000000000 ) ;
#8211 = EDGE_LOOP ( 'NONE', ( #8008, #3719, #7288, #2312, #6966 ) ) ;
#8212 = CARTESIAN_POINT ( 'NONE',  ( -91.33974596215564645, 171.6227766016838245, 0.000000000000000000 ) ) ;
#8213 = DIRECTION ( 'NONE',  ( -1.000000000000000000, -0.000000000000000000, -0.000000000000000000 ) ) ;
#8214 = FACE_OUTER_BOUND ( 'NONE', #16706, .T. ) ;
#8215 = FACE_OUTER_BOUND ( 'NONE', #12687, .T. ) ;
#8216 = CIRCLE ( 'NONE', #599, 2.499999999999998668 ) ;
#8217 = CARTESIAN_POINT ( 'NONE',  ( 25.87766738269516509, 137.9415577646583415, -9.529521052671011461 ) ) ;
#8218 = ORIENTED_EDGE ( 'NONE', *, *, #7565, .T. ) ;
#8219 = DIRECTION ( 'NONE',  ( 0.9961946980917464334, -0.04357787137382450326, 0.07547908730516456055 ) ) ;
#8220 = CARTESIAN_POINT ( 'NONE',  ( 15.56337975240378846, 125.2134999403455851, -5.000000000000001776 ) ) ;
#8221 = ORIENTED_EDGE ( 'NONE', *, *, #10404, .T. ) ;
#8222 = DIRECTION ( 'NONE',  ( 1.000000000000000000, 0.000000000000000000, 0.000000000000000000 ) ) ;
#8223 = CARTESIAN_POINT ( 'NONE',  ( -32.66708739526662697, 119.0939651702628623, -4.814896201988002389 ) ) ;
#8224 = CARTESIAN_POINT ( 'NONE',  ( 196.0000000000000000, 167.6227766016838814, -19.42820660268601074 ) ) ;
#8225 = APPLICATION_CONTEXT ( 'automotive_design' ) ;
#8226 = ADVANCED_FACE ( 'NONE', ( #13533 ), #10862, .T. ) ;
#8227 = CARTESIAN_POINT ( 'NONE',  ( -80.00000000000001421, 196.6227766016838245, -13.00000000000000000 ) ) ;
#8228 = ADVANCED_FACE ( 'NONE', ( #8214 ), #16372, .T. ) ;
#8229 = DIRECTION ( 'NONE',  ( -1.000000000000000000, 0.000000000000000000, -0.000000000000000000 ) ) ;
#8230 = CARTESIAN_POINT ( 'NONE',  ( 2.950000000000001066, 0.000000000000000000, 0.000000000000000000 ) ) ;
#8231 = AXIS2_PLACEMENT_3D ( 'NONE', #13047, #916, #3664 ) ;
#8232 = CARTESIAN_POINT ( 'NONE',  ( -45.00000000000000711, 171.6227766016838245, 0.000000000000000000 ) ) ;
#8233 = DIRECTION ( 'NONE',  ( 0.000000000000000000, -1.000000000000000000, 0.000000000000000000 ) ) ;
#8234 = DIRECTION ( 'NONE',  ( 0.000000000000000000, 0.000000000000000000, -1.000000000000000000 ) ) ;
#8235 = ORIENTED_EDGE ( 'NONE', *, *, #4592, .T. ) ;
#8236 = CARTESIAN_POINT ( 'NONE',  ( -14.83003349241641722, 19.99999999999883116, -8.298189366023557056 ) ) ;
#8237 = ORIENTED_EDGE ( 'NONE', *, *, #12607, .F. ) ;
#8238 = DIRECTION ( 'NONE',  ( -0.000000000000000000, -0.000000000000000000, -1.000000000000000000 ) ) ;
#8239 = ADVANCED_FACE ( 'NONE', ( #1571 ), #13358, .F. ) ;
#8240 = DIRECTION ( 'NONE',  ( -0.000000000000000000, -0.000000000000000000, 1.000000000000000000 ) ) ;
#8241 = ORIENTED_EDGE ( 'NONE', *, *, #14162, .F. ) ;
#8242 = FACE_OUTER_BOUND ( 'NONE', #2003, .T. ) ;
#8243 = CARTESIAN_POINT ( 'NONE',  ( 36.00000000000000711, 196.6227766016838245, -35.00000000000000000 ) ) ;
#8244 = B_SPLINE_CURVE_WITH_KNOTS ( 'NONE', 3,
 ( #5811, #1664, #5555, #1748, #8113, #2894, #12201, #4496, #10945, #2813, #11205, #4408, #16367, #15100 ),
 .UNSPECIFIED., .F., .F.,
 ( 4, 2, 2, 2, 2, 2, 4 ),
 ( 0.000000000000000000, 0.0006954478661160149247, 0.001043171799174032579, 0.001390895732232050232, 0.001738619665290067886, 0.002086343598348085540, 0.002781791464464176359 ),
 .UNSPECIFIED. ) ;
#8245 = ORIENTED_EDGE ( 'NONE', *, *, #12827, .T. ) ;
#8246 = CARTESIAN_POINT ( 'NONE',  ( 32.81385839426210538, 153.5807122668280158, -27.63145166803555597 ) ) ;
#8247 = ORIENTED_EDGE ( 'NONE', *, *, #8737, .F. ) ;
#8248 = DIRECTION ( 'NONE',  ( 0.000000000000000000, 0.000000000000000000, -1.000000000000000000 ) ) ;
#8249 = CARTESIAN_POINT ( 'NONE',  ( 15.56337975240373872, 125.2134999403456135, -4.999999999999997335 ) ) ;
#8250 = CARTESIAN_POINT ( 'NONE',  ( -40.00000000000000000, 0.000000000000000000, -33.00000000000000711 ) ) ;
#8251 = ORIENTED_EDGE ( 'NONE', *, *, #17473, .F. ) ;
#8252 = CARTESIAN_POINT ( 'NONE',  ( -50.00000000000000000, 171.6227766016838245, 0.000000000000000000 ) ) ;
#8253 = ORIENTED_EDGE ( 'NONE', *, *, #14772, .F. ) ;
#8254 = CARTESIAN_POINT ( 'NONE',  ( 25.53453899454350307, 148.8772865214096441, 23.90975478891752815 ) ) ;
#8255 = ORIENTED_EDGE ( 'NONE', *, *, #9290, .T. ) ;
#8256 = EDGE_CURVE ( 'NONE', #2414, #9987, #3980, .T. ) ;
#8257 = CARTESIAN_POINT ( 'NONE',  ( -86.98037184620996243, 193.8465113367683443, -24.40116746791569469 ) ) ;
#8258 = FACE_BOUND ( 'NONE', #3775, .T. ) ;
#8259 = ADVANCED_FACE ( 'NONE', ( #9367 ), #11392, .F. ) ;
#8260 = FACE_OUTER_BOUND ( 'NONE', #5336, .T. ) ;
#8261 = EDGE_LOOP ( 'NONE', ( #10168, #15508, #10574, #9977 ) ) ;
#8262 = EDGE_LOOP ( 'NONE', ( #6770, #13870 ) ) ;
#8263 = DIRECTION ( 'NONE',  ( -1.000000000000000000, -0.000000000000000000, -0.000000000000000000 ) ) ;
#8264 = CARTESIAN_POINT ( 'NONE',  ( 6.134011831684059501, 134.2062027339443944, 14.99999999999999822 ) ) ;
#8265 = VERTEX_POINT ( 'NONE', #12468 ) ;
#8266 = ADVANCED_FACE ( 'NONE', ( #335, #16800, #15105, #12374, #247, #8560, #3170, #3079, #2017, #3249, #8480, #414, #16460, #5820 ), #5652, .T. ) ;
#8267 = DIRECTION ( 'NONE',  ( -1.000000000000000000, 0.000000000000000000, 0.000000000000000000 ) ) ;
#8268 = DIRECTION ( 'NONE',  ( 0.000000000000000000, 0.000000000000000000, 1.000000000000000000 ) ) ;
#8269 = CARTESIAN_POINT ( 'NONE',  ( 18.00561851734427421, 29.93835620586352064, -12.40035566057732375 ) ) ;
#8270 = DIRECTION ( 'NONE',  ( -1.000000000000000000, 0.000000000000000000, 0.000000000000000000 ) ) ;
#8271 = CARTESIAN_POINT ( 'NONE',  ( -75.00000000000002842, 146.6227766016838245, 21.54065922853802562 ) ) ;
#8272 = EDGE_LOOP ( 'NONE', ( #10430, #13179 ) ) ;
#8273 = CARTESIAN_POINT ( 'NONE',  ( -84.31988691467586250, 200.8020376890377463, -19.33395870482236845 ) ) ;
#8274 = CARTESIAN_POINT ( 'NONE',  ( 15.00000000000000000, 171.6227766016838245, 20.00000000000000355 ) ) ;
#8275 = CARTESIAN_POINT ( 'NONE',  ( 19.49710218362280045, 19.99999999999999289, -24.48336163992366465 ) ) ;
#8276 = CARTESIAN_POINT ( 'NONE',  ( -39.68629150101524061, 122.0000000000000000, -9.686291501015231731 ) ) ;
#8277 = CARTESIAN_POINT ( 'NONE',  ( -157.2729844578908001, 171.6227766016837961, -126.3651973469810628 ) ) ;
#8278 = EDGE_LOOP ( 'NONE', ( #15389, #11150 ) ) ;
#8279 = CARTESIAN_POINT ( 'NONE',  ( -3.000000000000000888, 154.3022685259950038, -9.999999999999900524 ) ) ;
#8280 = ORIENTED_EDGE ( 'NONE', *, *, #3790, .F. ) ;
#8281 = CARTESIAN_POINT ( 'NONE',  ( -208.0000000000000853, 170.0678595944000620, -2.693195258168412654 ) ) ;
#8282 = ORIENTED_EDGE ( 'NONE', *, *, #15869, .F. ) ;
#8283 = EDGE_CURVE ( 'NONE', #11917, #11907, #5736, .T. ) ;
#8284 =( NAMED_UNIT ( * ) SI_UNIT ( $, .STERADIAN. ) SOLID_ANGLE_UNIT ( ) );
#8285 = EDGE_CURVE ( 'NONE', #1227, #10007, #4413, .T. ) ;
#8286 = CARTESIAN_POINT ( 'NONE',  ( 27.47046887371370616, 136.6950068244141221, -2.596529902249163690 ) ) ;
#8287 = ADVANCED_FACE ( 'NONE', ( #4667 ), #605, .T. ) ;
#8288 = FILL_AREA_STYLE ('',( #13887 ) ) ;
#8289 = CARTESIAN_POINT ( 'NONE',  ( -73.00000000000001421, 171.6227766016838245, 0.000000000000000000 ) ) ;
#8290 = ORIENTED_EDGE ( 'NONE', *, *, #14847, .T. ) ;
#8291 = CARTESIAN_POINT ( 'NONE',  ( -138.7106781186547266, 171.6227766016838245, -2.296212748401287183E-15 ) ) ;
#8292 = DIRECTION ( 'NONE',  ( 0.000000000000000000, 0.000000000000000000, 1.000000000000000000 ) ) ;
#8293 = CARTESIAN_POINT ( 'NONE',  ( -80.00000000000002842, 146.6227766016838245, -16.00000000000000000 ) ) ;
#8294 = CARTESIAN_POINT ( 'NONE',  ( 16.01769397135448614, 136.8393535285713369, -3.937079669079308175 ) ) ;
#8295 = VERTEX_POINT ( 'NONE', #9709 ) ;
#8296 = DIRECTION ( 'NONE',  ( 0.000000000000000000, 0.000000000000000000, 1.000000000000000000 ) ) ;
#8297 = DIRECTION ( 'NONE',  ( 0.000000000000000000, 0.000000000000000000, 1.000000000000000000 ) ) ;
#8298 = ORIENTED_EDGE ( 'NONE', *, *, #6199, .F. ) ;
#8299 = EDGE_CURVE ( 'NONE', #13669, #2967, #12548, .T. ) ;
#8300 = CARTESIAN_POINT ( 'NONE',  ( -78.20073929934177670, 190.8809388003085417, -29.22564348704268511 ) ) ;
#8301 = LINE ( 'NONE', #14952, #1084 ) ;
#8302 = CARTESIAN_POINT ( 'NONE',  ( 26.34659224751355211, 193.1938012187558797, 24.97603563008314254 ) ) ;
#8303 = FACE_OUTER_BOUND ( 'NONE', #15199, .T. ) ;
#8304 = CARTESIAN_POINT ( 'NONE',  ( 196.0000000000000000, 171.6227766016838245, -12.50000337241049131 ) ) ;
#8305 = CARTESIAN_POINT ( 'NONE',  ( 21.87945022329474298, 29.86245334106958538, 9.005757899690800983 ) ) ;
#8306 = DIRECTION ( 'NONE',  ( 0.000000000000000000, 0.000000000000000000, -1.000000000000000000 ) ) ;
#8307 = CARTESIAN_POINT ( 'NONE',  ( -168.0000000000000284, 168.3180863238818006, -5.723891464432168341 ) ) ;
#8308 = AXIS2_PLACEMENT_3D ( 'NONE', #6347, #8912, #3783 ) ;
#8309 = ORIENTED_EDGE ( 'NONE', *, *, #5217, .F. ) ;
#8310 = CARTESIAN_POINT ( 'NONE',  ( -11.99122994684825549, 19.99999999999999645, -24.50500383881168176 ) ) ;
#8311 = VECTOR ( 'NONE', #11174, 1000.000000000000000 ) ;
#8312 = ORIENTED_EDGE ( 'NONE', *, *, #624, .T. ) ;
#8313 = CARTESIAN_POINT ( 'NONE',  ( -7.379000772445021283, 30.00000000000000000, 13.00000000000000000 ) ) ;
#8314 = CARTESIAN_POINT ( 'NONE',  ( -95.00000000000000000, 171.6227766016838245, 0.000000000000000000 ) ) ;
#8315 = ORIENTED_EDGE ( 'NONE', *, *, #9520, .T. ) ;
#8316 = EDGE_CURVE ( 'NONE', #15643, #17487, #1927, .T. ) ;
#8317 = CARTESIAN_POINT ( 'NONE',  ( -21.36854569161992856, 19.99999999999999645, 19.70709815271291632 ) ) ;
#8318 = FACE_OUTER_BOUND ( 'NONE', #674, .T. ) ;
#8319 = ORIENTED_EDGE ( 'NONE', *, *, #11083, .T. ) ;
#8320 = CARTESIAN_POINT ( 'NONE',  ( 33.07446265461972956, 153.4692325703934159, -27.55849099911372591 ) ) ;
#8321 = AXIS2_PLACEMENT_3D ( 'NONE', #11079, #2936, #4025 ) ;
#8322 = ORIENTED_EDGE ( 'NONE', *, *, #1653, .T. ) ;
#8324 = B_SPLINE_CURVE_WITH_KNOTS ( 'NONE', 3,
 ( #14168, #701, #6269, #17151, #15570, #16991, #15647, #7421, #6093, #1043, #5026, #11492, #4858, #3617, #10248, #10510, #952, #7677, #16901, #3447 ),
 .UNSPECIFIED., .F., .F.,
 ( 4, 2, 2, 2, 2, 2, 2, 2, 2, 4 ),
 ( 0.000000000000000000, 0.002053780611527093129, 0.004107561223054186257, 0.006161341834581279819, 0.008215122446108372514, 0.01026890305763546694, 0.01232268366916255964, 0.01437646428068965233, 0.01540335458645322037, 0.01643024489221679013 ),
 .UNSPECIFIED. ) ;
#8323 = CARTESIAN_POINT ( 'NONE',  ( -25.81010901361623056, 18.00000000000000000, 13.97188021846430139 ) ) ;
#8325 = CIRCLE ( 'NONE', #16821, 20.00000000000000355 ) ;
#8326 = DIRECTION ( 'NONE',  ( 0.000000000000000000, 0.000000000000000000, 1.000000000000000000 ) ) ;
#8327 = DIRECTION ( 'NONE',  ( -1.156482317317868274E-16, 1.000000000000000000, 0.000000000000000000 ) ) ;
#8328 = CARTESIAN_POINT ( 'NONE',  ( -70.00000000000000000, 143.0439382767972631, 16.49999999999984013 ) ) ;
#8329 = ORIENTED_EDGE ( 'NONE', *, *, #5051, .T. ) ;
#8330 = CYLINDRICAL_SURFACE ( 'NONE', #1258, 5.000000000000004441 ) ;
#8331 = DIRECTION ( 'NONE',  ( -1.000000000000000000, 0.000000000000000000, 0.000000000000000000 ) ) ;
#8332 = ORIENTED_EDGE ( 'NONE', *, *, #8571, .T. ) ;
#8333 = CARTESIAN_POINT ( 'NONE',  ( 27.19159743497788284, 137.1791639268274992, -6.327035192214271575 ) ) ;
#8334 = ORIENTED_EDGE ( 'NONE', *, *, #15065, .T. ) ;
#8335 = CARTESIAN_POINT ( 'NONE',  ( -83.81731182140758563, 190.1433283039765172, -27.31438289289431509 ) ) ;
#8336 = CARTESIAN_POINT ( 'NONE',  ( -77.50000000000001421, 196.6227766016838245, 1.387778780781445676E-14 ) ) ;
#8337 = VECTOR ( 'NONE', #9177, 1000.000000000000000 ) ;
#8338 = CARTESIAN_POINT ( 'NONE',  ( -7.922882945419460476, 30.18055256556250399, -13.00000000000000355 ) ) ;
#8339 = ORIENTED_EDGE ( 'NONE', *, *, #3064, .F. ) ;
#8340 = VERTEX_POINT ( 'NONE', #4501 ) ;
#8341 = EDGE_CURVE ( 'NONE', #10145, #5870, #9892, .T. ) ;
#8342 = CYLINDRICAL_SURFACE ( 'NONE', #16847, 5.000000000000018652 ) ;
#8343 = AXIS2_PLACEMENT_3D ( 'NONE', #1511, #10978, #12306 ) ;
#8344 = FACE_OUTER_BOUND ( 'NONE', #3994, .T. ) ;
#8345 = CARTESIAN_POINT ( 'NONE',  ( 11.61835878478676598, 131.7755375868723320, 13.65455057792075877 ) ) ;
#8346 = VERTEX_POINT ( 'NONE', #3348 ) ;
#8347 = CONTEXT_DEPENDENT_SHAPE_REPRESENTATION ( #10024, #16636 ) ;
#8348 = DIRECTION ( 'NONE',  ( 0.000000000000000000, 0.000000000000000000, 1.000000000000000000 ) ) ;
#8349 = EDGE_CURVE ( 'NONE', #11303, #1820, #13804, .T. ) ;
#8350 = CYLINDRICAL_SURFACE ( 'NONE', #13454, 39.99999999999997868 ) ;
#8351 = ADVANCED_FACE ( 'NONE', ( #1669 ), #13971, .T. ) ;
#8352 = AXIS2_PLACEMENT_3D ( 'NONE', #5466, #4140, #9526 ) ;
#8353 = DIRECTION ( 'NONE',  ( 1.000000000000000000, 0.000000000000000000, 0.000000000000000000 ) ) ;
#8354 = CARTESIAN_POINT ( 'NONE',  ( 34.93420767853316988, 19.99999999999999645, 0.000000000000000000 ) ) ;
#8355 = CARTESIAN_POINT ( 'NONE',  ( -725.0000000000000000, 19.99999999999995737, 15.00000000000000000 ) ) ;
#8356 = VECTOR ( 'NONE', #5375, 1000.000000000000000 ) ;
#8357 = EDGE_LOOP ( 'NONE', ( #9219, #8485 ) ) ;
#8358 = CARTESIAN_POINT ( 'NONE',  ( -32.34996859905195521, 100.2591029109095189, 5.378151393592374596 ) ) ;
#8359 = VECTOR ( 'NONE', #13021, 1000.000000000000000 ) ;
#8360 = DIRECTION ( 'NONE',  ( 0.000000000000000000, 0.000000000000000000, -1.000000000000000000 ) ) ;
#8361 = CARTESIAN_POINT ( 'NONE',  ( 0.000000000000000000, -0.8660254037844428154, 1.500000000000001332 ) ) ;
#8362 = DIRECTION ( 'NONE',  ( 0.9961946980917465444, 0.08715574274764831264, 0.000000000000000000 ) ) ;
#8363 = LINE ( 'NONE', #1650, #14311 ) ;
#8364 = PRODUCT_DEFINITION_CONTEXT ( 'detailed design', #86, 'design' ) ;
#8365 = EDGE_LOOP ( 'NONE', ( #11702, #13362, #11371, #15316, #462, #6499 ) ) ;
#8366 = ORIENTED_EDGE ( 'NONE', *, *, #8124, .T. ) ;
#8367 = CIRCLE ( 'NONE', #6684, 25.00000000000000000 ) ;
#8368 = CARTESIAN_POINT ( 'NONE',  ( -147.9615242270661213, 171.6227766016838245, 0.000000000000000000 ) ) ;
#8369 = AXIS2_PLACEMENT_3D ( 'NONE', #3944, #2334, #923 ) ;
#8370 = ORIENTED_EDGE ( 'NONE', *, *, #16219, .T. ) ;
#8371 = FACE_OUTER_BOUND ( 'NONE', #5527, .T. ) ;
#8372 = VERTEX_POINT ( 'NONE', #11124 ) ;
#8373 =( LENGTH_UNIT ( ) NAMED_UNIT ( * ) SI_UNIT ( .MILLI., .METRE. ) );
#8374 = CARTESIAN_POINT ( 'NONE',  ( -35.49999999999998579, 10.00000000000000178, -13.00000000000000000 ) ) ;
#8375 = FACE_OUTER_BOUND ( 'NONE', #12203, .T. ) ;
#8376 = DIRECTION ( 'NONE',  ( -0.000000000000000000, -0.000000000000000000, -1.000000000000000000 ) ) ;
#8377 = CARTESIAN_POINT ( 'NONE',  ( 37.50000000000000711, 146.6227766016838245, -21.54065922853802562 ) ) ;
#8378 = AXIS2_PLACEMENT_3D ( 'NONE', #14880, #9561, #13729 ) ;
#8379 = CIRCLE ( 'NONE', #10070, 5.000000000000018652 ) ;
#8380 = VERTEX_POINT ( 'NONE', #7234 ) ;
#8381 = FACE_OUTER_BOUND ( 'NONE', #9058, .T. ) ;
#8382 = FACE_OUTER_BOUND ( 'NONE', #4345, .T. ) ;
#8383 = AXIS2_PLACEMENT_3D ( 'NONE', #10528, #8048, #13287 ) ;
#8384 = CARTESIAN_POINT ( 'NONE',  ( -3.000000000000000888, 171.6227766016838245, 0.000000000000000000 ) ) ;
#8385 = CYLINDRICAL_SURFACE ( 'NONE', #15137, 2.500000000000000444 ) ;
#8386 = AXIS2_PLACEMENT_3D ( 'NONE', #2825, #6891, #11050 ) ;
#8387 = ADVANCED_FACE ( 'NONE', ( #14152 ), #12638, .T. ) ;
#8388 = EDGE_CURVE ( 'NONE', #2665, #12251, #4589, .T. ) ;
#8389 = CARTESIAN_POINT ( 'NONE',  ( 27.25143353317894324, 137.1251711682953385, -6.002437647192902404 ) ) ;
#8390 = ORIENTED_EDGE ( 'NONE', *, *, #14232, .F. ) ;
#8391 = FACE_BOUND ( 'NONE', #3531, .T. ) ;
#8392 = CARTESIAN_POINT ( 'NONE',  ( 13.73607130285369138, 138.7967234794426190, -3.453855393587564659 ) ) ;
#8393 = ORIENTED_EDGE ( 'NONE', *, *, #2877, .T. ) ;
#8394 = AXIS2_PLACEMENT_3D ( 'NONE', #1336, #1941, #5836 ) ;
#8395 = CARTESIAN_POINT ( 'NONE',  ( -74.00000000000001421, 195.9827547425045680, -25.14811700250532311 ) ) ;
#8396 = STYLED_ITEM ( 'NONE', ( #12723 ), #9102 ) ;
#8397 = VECTOR ( 'NONE', #12995, 1000.000000000000000 ) ;
#8398 = CYLINDRICAL_SURFACE ( 'NONE', #6742, 2.500000000000000444 ) ;
#8399 = DIRECTION ( 'NONE',  ( 0.000000000000000000, 0.000000000000000000, 1.000000000000000000 ) ) ;
#8400 = CARTESIAN_POINT ( 'NONE',  ( -90.80384757729339640, 204.6227766016838245, 0.000000000000000000 ) ) ;
#8401 = LINE ( 'NONE', #12483, #12358 ) ;
#8402 = CARTESIAN_POINT ( 'NONE',  ( 16.75836516268004317, 29.96322345091821049, 12.79344305462037035 ) ) ;
#8403 = CARTESIAN_POINT ( 'NONE',  ( -84.59204834251386274, 198.6215000397446886, 18.98099903503496577 ) ) ;
#8404 = ORIENTED_EDGE ( 'NONE', *, *, #9479, .T. ) ;
#8405 = EDGE_CURVE ( 'NONE', #2271, #7472, #12743, .T. ) ;
#8406 = EDGE_CURVE ( 'NONE', #2141, #10037, #15899, .T. ) ;
#8407 = VECTOR ( 'NONE', #10950, 1000.000000000000000 ) ;
#8408 = ADVANCED_FACE ( 'NONE', ( #17051 ), #13074, .F. ) ;
#8409 = ORIENTED_EDGE ( 'NONE', *, *, #13073, .T. ) ;
#8410 = VERTEX_POINT ( 'NONE', #13187 ) ;
#8411 = CARTESIAN_POINT ( 'NONE',  ( -40.00000000000000000, 4.000000000000000000, 33.00000000000000711 ) ) ;
#8412 = EDGE_CURVE ( 'NONE', #6662, #14433, #8125, .T. ) ;
#8413 = ORIENTED_EDGE ( 'NONE', *, *, #5126, .F. ) ;
#8414 = CARTESIAN_POINT ( 'NONE',  ( -151.6393416600920716, 171.6227766016838245, 0.000000000000000000 ) ) ;
#8415 = DIRECTION ( 'NONE',  ( -1.000000000000000000, 0.000000000000000000, 0.000000000000000000 ) ) ;
#8416 = VERTEX_POINT ( 'NONE', #8990 ) ;
#8417 = PRODUCT ( '3-Stage Planetary Gearbox', '3-Stage Planetary Gearbox', '', ( #9766 ) ) ;
#8418 = CARTESIAN_POINT ( 'NONE',  ( 25.75320729262171682, 152.8105824767976060, -27.11332964807918344 ) ) ;
#8419 = FACE_OUTER_BOUND ( 'NONE', #14217, .T. ) ;
#8420 = VECTOR ( 'NONE', #12984, 1000.000000000000000 ) ;
#8421 = CIRCLE ( 'NONE', #12955, 6.000000000000005329 ) ;
#8422 = FACE_OUTER_BOUND ( 'NONE', #2647, .T. ) ;
#8423 = CARTESIAN_POINT ( 'NONE',  ( 17.00000000000000000, 171.6227766016838245, 0.000000000000000000 ) ) ;
#8424 = CYLINDRICAL_SURFACE ( 'NONE', #15797, 20.00000000000000355 ) ;
#8425 = LINE ( 'NONE', #13844, #14259 ) ;
#8426 = ADVANCED_FACE ( 'NONE', ( #11474 ), #4761, .T. ) ;
#8427 = PLANE ( 'NONE',  #7195 ) ;
#8428 = B_SPLINE_CURVE_WITH_KNOTS ( 'NONE', 3,
 ( #4660, #1916, #16970, #7319, #3502, #12725, #597, #7404, #11386, #15459, #677, #11467, #11559, #16879, #4752, #10142, #15547, #2084, #767, #6163 ),
 .UNSPECIFIED., .F., .F.,
 ( 4, 2, 2, 2, 2, 2, 2, 2, 2, 4 ),
 ( 0.000000000000000000, 0.002053780611527093129, 0.004107561223054186257, 0.006161341834581279819, 0.008215122446108372514, 0.01026890305763546694, 0.01232268366916255964, 0.01437646428068965233, 0.01540335458645322037, 0.01643024489221679013 ),
 .UNSPECIFIED. ) ;
#8429 = EDGE_LOOP ( 'NONE', ( #3278, #14235, #2222, #4975, #13828, #4557 ) ) ;
#8430 = FACE_OUTER_BOUND ( 'NONE', #5000, .T. ) ;
#8431 = EDGE_LOOP ( 'NONE', ( #12713, #6982, #4399, #6348, #7976 ) ) ;
#8432 = CARTESIAN_POINT ( 'NONE',  ( -45.00000000000000711, 171.6227766016838245, 19.49999999999998224 ) ) ;
#8433 = DIRECTION ( 'NONE',  ( 1.000000000000000000, 0.000000000000000000, 0.000000000000000000 ) ) ;
#8434 = CARTESIAN_POINT ( 'NONE',  ( 48.00000000000000711, 163.6227766016838530, -10.00000337241049309 ) ) ;
#8435 = AXIS2_PLACEMENT_3D ( 'NONE', #12328, #4105, #9489 ) ;
#8436 = EDGE_LOOP ( 'NONE', ( #2035, #6574, #6314, #11975 ) ) ;
#8437 = VERTEX_POINT ( 'NONE', #3511 ) ;
#8438 = FACE_OUTER_BOUND ( 'NONE', #10075, .T. ) ;
#8439 = VECTOR ( 'NONE', #6805, 1000.000000000000114 ) ;
#8440 = DIRECTION ( 'NONE',  ( 0.000000000000000000, -1.000000000000000000, 0.000000000000000000 ) ) ;
#8441 = FACE_OUTER_BOUND ( 'NONE', #16137, .T. ) ;
#8442 = ORIENTED_EDGE ( 'NONE', *, *, #7355, .T. ) ;
#8443 = CONTEXT_DEPENDENT_SHAPE_REPRESENTATION ( #10140, #8123 ) ;
#8444 = DIRECTION ( 'NONE',  ( 1.000000000000000000, 0.000000000000000000, 0.000000000000000000 ) ) ;
#8445 = CARTESIAN_POINT ( 'NONE',  ( 48.00000000000000711, 167.6227766016838530, -5.571800142134975431 ) ) ;
#8446 = CARTESIAN_POINT ( 'NONE',  ( 19.82112781281243130, 29.90253658286262350, -11.35562597552217845 ) ) ;
#8447 = VECTOR ( 'NONE', #5299, 1000.000000000000000 ) ;
#8448 = CARTESIAN_POINT ( 'NONE',  ( -100.0000000000000000, 171.6227766016838245, 0.000000000000000000 ) ) ;
#8449 = EDGE_CURVE ( 'NONE', #17341, #3275, #11565, .T. ) ;
#8450 = FACE_OUTER_BOUND ( 'NONE', #1842, .T. ) ;
#8451 = CIRCLE ( 'NONE', #10712, 239.9999999999999716 ) ;
#8452 = CARTESIAN_POINT ( 'NONE',  ( -13.90980987654335976, 19.99999999999998934, 23.98326992096530219 ) ) ;
#8453 = EDGE_CURVE ( 'NONE', #5896, #16720, #7487, .T. ) ;
#8454 = ORIENTED_EDGE ( 'NONE', *, *, #5217, .T. ) ;
#8455 = CARTESIAN_POINT ( 'NONE',  ( 48.00000000000000711, 163.6227766016838530, 12.50000337241049309 ) ) ;
#8456 = FACE_OUTER_BOUND ( 'NONE', #11793, .T. ) ;
#8457 = CARTESIAN_POINT ( 'NONE',  ( -725.0000000000000000, 19.99999999999995737, 15.00000000000000000 ) ) ;
#8458 = CYLINDRICAL_SURFACE ( 'NONE', #14954, 8.000000000000000000 ) ;
#8459 = LINE ( 'NONE', #4128, #11196 ) ;
#8460 = ORIENTED_EDGE ( 'NONE', *, *, #2896, .T. ) ;
#8461 = ORIENTED_EDGE ( 'NONE', *, *, #7277, .T. ) ;
#8462 = ADVANCED_FACE ( 'NONE', ( #17223 ), #11723, .F. ) ;
#8463 = ADVANCED_FACE ( 'NONE', ( #14307 ), #6330, .T. ) ;
#8464 = VECTOR ( 'NONE', #14062, 1000.000000000000000 ) ;
#8465 = CARTESIAN_POINT ( 'NONE',  ( 10.91733900447548322, 143.9222794873857652, 17.93588862913478366 ) ) ;
#8466 = VECTOR ( 'NONE', #2841, 1000.000000000000000 ) ;
#8467 = ORIENTED_EDGE ( 'NONE', *, *, #15639, .T. ) ;
#8468 = CARTESIAN_POINT ( 'NONE',  ( 27.48361012698968864, 136.6227766016838245, 0.000000000000000000 ) ) ;
#8469 = AXIS2_PLACEMENT_3D ( 'NONE', #12598, #15160, #9940 ) ;
#8470 = VERTEX_POINT ( 'NONE', #774 ) ;
#8471 = DIRECTION ( 'NONE',  ( -1.000000000000000000, 0.000000000000000000, 0.000000000000000000 ) ) ;
#8472 =( LENGTH_UNIT ( ) NAMED_UNIT ( * ) SI_UNIT ( .MILLI., .METRE. ) );
#8473 = DIRECTION ( 'NONE',  ( -1.000000000000000000, 0.000000000000000000, 0.000000000000000000 ) ) ;
#8474 = LINE ( 'NONE', #408, #16280 ) ;
#8475 = CARTESIAN_POINT ( 'NONE',  ( 22.65507808637627818, 17.99999999999885958, -7.619675430596801746 ) ) ;
#8476 = VERTEX_POINT ( 'NONE', #2179 ) ;
#8477 = CARTESIAN_POINT ( 'NONE',  ( 30.91638155568829660, 141.7021811473759669, 13.91989935049638305 ) ) ;
#8478 = CIRCLE ( 'NONE', #8766, 10.00000000000000178 ) ;
#8479 = DIRECTION ( 'NONE',  ( 0.000000000000000000, 0.000000000000000000, -1.000000000000000000 ) ) ;
#8480 = FACE_BOUND ( 'NONE', #12643, .T. ) ;
#8481 = CIRCLE ( 'NONE', #9040, 2.500000000000002220 ) ;
#8482 = DIRECTION ( 'NONE',  ( -0.000000000000000000, -0.000000000000000000, -1.000000000000000000 ) ) ;
#8483 = EDGE_CURVE ( 'NONE', #10629, #5121, #4541, .T. ) ;
#8484 = CARTESIAN_POINT ( 'NONE',  ( 48.00000000000000711, 163.6227766016838530, 10.00000337241049309 ) ) ;
#8485 = ORIENTED_EDGE ( 'NONE', *, *, #5899, .F. ) ;
#8486 = CARTESIAN_POINT ( 'NONE',  ( 48.00000000000000711, 187.6227766016837961, -12.50000337241049309 ) ) ;
#8487 = CIRCLE ( 'NONE', #10752, 1.500000000000000000 ) ;
#8488 = AXIS2_PLACEMENT_3D ( 'NONE', #6170, #15558, #8899 ) ;
#8489 = VERTEX_POINT ( 'NONE', #3598 ) ;
#8490 = CARTESIAN_POINT ( 'NONE',  ( -74.60025079181714602, 194.0006876528842383, -26.91236748077486141 ) ) ;
#8491 = FACE_OUTER_BOUND ( 'NONE', #11757, .T. ) ;
#8492 = EDGE_CURVE ( 'NONE', #2208, #4989, #6425, .T. ) ;
#8493 = CARTESIAN_POINT ( 'NONE',  ( 25.08013182200793878, 195.5664139939901816, 22.72185355927996042 ) ) ;
#8494 = FACE_OUTER_BOUND ( 'NONE', #10932, .T. ) ;
#8495 = DIRECTION ( 'NONE',  ( 1.000000000000000000, 0.000000000000000000, 0.000000000000000000 ) ) ;
#8496 = CARTESIAN_POINT ( 'NONE',  ( 22.51550247401197069, 29.85017970947654575, 7.570302168957804057 ) ) ;
#8497 = CARTESIAN_POINT ( 'NONE',  ( -77.77775085091418816, 201.1051302811612231, 14.82644580554059743 ) ) ;
#8498 = FACE_BOUND ( 'NONE', #9099, .T. ) ;
#8499 = ORIENTED_EDGE ( 'NONE', *, *, #7801, .T. ) ;
#8500 = AXIS2_PLACEMENT_3D ( 'NONE', #16574, #4933, #12671 ) ;
#8501 = ORIENTED_EDGE ( 'NONE', *, *, #2294, .T. ) ;
#8502 = CARTESIAN_POINT ( 'NONE',  ( 34.93420767853316988, 30.00000000000000000, 15.00000000000000000 ) ) ;
#8503 = CIRCLE ( 'NONE', #6819, 20.00000000000000355 ) ;
#8504 = DIRECTION ( 'NONE',  ( -1.000000000000000000, 0.000000000000000000, 0.000000000000000000 ) ) ;
#8505 = VERTEX_POINT ( 'NONE', #7663 ) ;
#8506 = DIRECTION ( 'NONE',  ( -3.469446951953613696E-16, 1.000000000000000000, -0.000000000000000000 ) ) ;
#8507 = DIRECTION ( 'NONE',  ( 0.000000000000000000, 0.000000000000000000, 1.000000000000000000 ) ) ;
#8508 = VERTEX_POINT ( 'NONE', #11649 ) ;
#8509 = CARTESIAN_POINT ( 'NONE',  ( 36.65543510501046143, 200.1146145092351958, -16.67123533649926870 ) ) ;
#8510 = AXIS2_PLACEMENT_3D ( 'NONE', #5072, #15524, #10471 ) ;
#8511 = CARTESIAN_POINT ( 'NONE',  ( -157.2729844578908001, 171.6227766016838245, 126.3651973469810628 ) ) ;
#8512 = EDGE_CURVE ( 'NONE', #4546, #12075, #4919, .T. ) ;
#8513 = EDGE_CURVE ( 'NONE', #4855, #190, #14993, .T. ) ;
#8514 = EDGE_CURVE ( 'NONE', #8812, #8947, #11593, .T. ) ;
#8515 = CARTESIAN_POINT ( 'NONE',  ( -75.00000000000002842, 146.6227766016838245, -12.99999999999999822 ) ) ;
#8516 = FACE_OUTER_BOUND ( 'NONE', #9693, .T. ) ;
#8517 = CARTESIAN_POINT ( 'NONE',  ( -20.00000000000000355, 171.6227766016838245, -19.49999999999998934 ) ) ;
#8518 = LINE ( 'NONE', #12502, #17085 ) ;
#8519 = DIRECTION ( 'NONE',  ( 0.000000000000000000, 0.000000000000000000, -1.000000000000000000 ) ) ;
#8520 = EDGE_LOOP ( 'NONE', ( #11795, #4134, #12539 ) ) ;
#8521 = CARTESIAN_POINT ( 'NONE',  ( 26.38776508739448801, 137.6838126476015134, -8.633687169601740763 ) ) ;
#8522 = VERTEX_POINT ( 'NONE', #14484 ) ;
#8523 = CARTESIAN_POINT ( 'NONE',  ( 27.47054928355543169, 136.6945666198121216, 2.592592592592591672 ) ) ;
#8524 = AXIS2_PLACEMENT_3D ( 'NONE', #4278, #7016, #7272 ) ;
#8525 = CARTESIAN_POINT ( 'NONE',  ( -12.54777316999452275, 31.64944667534048861, -11.54374194473465920 ) ) ;
#8526 = ORIENTED_EDGE ( 'NONE', *, *, #5496, .F. ) ;
#8527 = ORIENTED_EDGE ( 'NONE', *, *, #10443, .T. ) ;
#8528 = DIRECTION ( 'NONE',  ( 0.000000000000000000, 8.410780489584519664E-16, 1.000000000000000000 ) ) ;
#8529 = CARTESIAN_POINT ( 'NONE',  ( 49.99999999999998579, 187.6227766016837961, 10.00000337241049309 ) ) ;
#8530 = CARTESIAN_POINT ( 'NONE',  ( 16.64812168497169864, 126.9869021000460663, 8.626120676703536105 ) ) ;
#8531 = VERTEX_POINT ( 'NONE', #5102 ) ;
#8532 = ITEM_DEFINED_TRANSFORMATION ( 'NONE', 'NONE', #10676,  #3583 ) ;
#8533 = DIRECTION ( 'NONE',  ( 0.000000000000000000, 0.000000000000000000, -1.000000000000000000 ) ) ;
#8534 = CYLINDRICAL_SURFACE ( 'NONE', #13173, 5.000000000000007994 ) ;
#8535 = CARTESIAN_POINT ( 'NONE',  ( -82.86886491573849867, 192.5125816722295724, 25.54797519334867673 ) ) ;
#8536 = CARTESIAN_POINT ( 'NONE',  ( 15.60228996708978855, 124.9392590763941371, -1.387778780781445676E-14 ) ) ;
#8537 = CARTESIAN_POINT ( 'NONE',  ( 17.58250999373992585, 125.2198453306090329, -1.325401613797208934E-14 ) ) ;
#8538 = CARTESIAN_POINT ( 'NONE',  ( 196.0000000000000000, 191.6227766016837677, 5.571800142134975431 ) ) ;
#8539 = EDGE_LOOP ( 'NONE', ( #1081, #14176, #8035, #12509 ) ) ;
#8540 = CARTESIAN_POINT ( 'NONE',  ( -75.66955265303195688, 200.7908024820230253, -19.35080275744227407 ) ) ;
#8541 = DIRECTION ( 'NONE',  ( -1.000000000000000000, -0.000000000000000000, 0.000000000000000000 ) ) ;
#8542 = LINE ( 'NONE', #8361, #818 ) ;
#8543 = CARTESIAN_POINT ( 'NONE',  ( -73.00000000000001421, 171.6227766016838245, 0.000000000000000000 ) ) ;
#8544 = CARTESIAN_POINT ( 'NONE',  ( 49.99999999999998579, 151.6227766016839098, 8.071800142134973655 ) ) ;
#8545 = ORIENTED_EDGE ( 'NONE', *, *, #10597, .F. ) ;
#8546 = ORIENTED_EDGE ( 'NONE', *, *, #5922, .F. ) ;
#8547 = VERTEX_POINT ( 'NONE', #3769 ) ;
#8548 = CARTESIAN_POINT ( 'NONE',  ( 6.134011831684053284, 134.2062027339443944, -15.00000000000000000 ) ) ;
#8549 = ORIENTED_EDGE ( 'NONE', *, *, #12704, .F. ) ;
#8550 = ADVANCED_FACE ( 'NONE', ( #9163 ), #14569, .F. ) ;
#8551 = DIRECTION ( 'NONE',  ( -1.000000000000000000, -0.000000000000000000, -0.000000000000000000 ) ) ;
#8552 = ORIENTED_EDGE ( 'NONE', *, *, #10374, .T. ) ;
#8553 =( NAMED_UNIT ( * ) PLANE_ANGLE_UNIT ( ) SI_UNIT ( $, .RADIAN. ) );
#8554 = DIRECTION ( 'NONE',  ( -0.000000000000000000, -0.000000000000000000, 1.000000000000000000 ) ) ;
#8555 = CARTESIAN_POINT ( 'NONE',  ( -27.99999999999998224, 10.00000000000000000, 0.000000000000000000 ) ) ;
#8556 = DIRECTION ( 'NONE',  ( -0.000000000000000000, -0.000000000000000000, 1.000000000000000000 ) ) ;
#8557 = ORIENTED_EDGE ( 'NONE', *, *, #719, .F. ) ;
#8558 = CARTESIAN_POINT ( 'NONE',  ( 34.20572221690138548, 143.8556217771935053, 17.85322440072383543 ) ) ;
#8559 = DIRECTION ( 'NONE',  ( -1.000000000000000000, -0.000000000000000000, -0.000000000000000000 ) ) ;
#8560 = FACE_BOUND ( 'NONE', #17483, .T. ) ;
#8561 = CARTESIAN_POINT ( 'NONE',  ( -725.0000000000000000, 19.99999999999995737, -15.00000000000000000 ) ) ;
#8562 = PRODUCT_DEFINITION_SHAPE ( 'NONE', 'NONE',  #17525 ) ;
#8563 = DIRECTION ( 'NONE',  ( 0.9961946980917463224, -0.04357787137382344855, -0.07547908730516518505 ) ) ;
#8564 = ORIENTED_EDGE ( 'NONE', *, *, #3503, .T. ) ;
#8565 = EDGE_CURVE ( 'NONE', #12513, #1130, #1117, .T. ) ;
#8566 = CARTESIAN_POINT ( 'NONE',  ( 27.47054928355543169, 136.6945666198121216, -2.592592592592591672 ) ) ;
#8567 = ORIENTED_EDGE ( 'NONE', *, *, #15097, .F. ) ;
#8568 = SURFACE_STYLE_USAGE ( .BOTH. , #11319 ) ;
#8569 = CARTESIAN_POINT ( 'NONE',  ( 17.91514137517177474, 140.8731888928338094, 16.72020691847105667 ) ) ;
#8570 = DIRECTION ( 'NONE',  ( 1.000000000000000000, 0.000000000000000000, 0.000000000000000000 ) ) ;
#8571 = EDGE_CURVE ( 'NONE', #3946, #14086, #14431, .T. ) ;
#8572 = CARTESIAN_POINT ( 'NONE',  ( 28.65205091688542893, 191.8039921295446106, 26.10980206683225902 ) ) ;
#8573 = EDGE_CURVE ( 'NONE', #5381, #8372, #6793, .T. ) ;
#8574 = CARTESIAN_POINT ( 'NONE',  ( -24.93725393319378725, 100.0000000000000142, -5.500000000000000000 ) ) ;
#8575 = EDGE_CURVE ( 'NONE', #8489, #9733, #1048, .T. ) ;
#8576 = CARTESIAN_POINT ( 'NONE',  ( -725.0000000000000000, 19.99999999999995737, -4.999999999999999112 ) ) ;
#8577 = CYLINDRICAL_SURFACE ( 'NONE', #14667, 8.000000000000000000 ) ;
#8578 = CARTESIAN_POINT ( 'NONE',  ( -82.70586383762018556, 200.8416626254457640, 15.34246182976911932 ) ) ;
#8579 = DIRECTION ( 'NONE',  ( 0.9961946980917464334, -0.04357787137382345549, -0.07547908730516519893 ) ) ;
#8580 = VERTEX_POINT ( 'NONE', #2438 ) ;
#8581 = EDGE_CURVE ( 'NONE', #12327, #9960, #301, .T. ) ;
#8582 = VERTEX_POINT ( 'NONE', #10577 ) ;
#8583 = CARTESIAN_POINT ( 'NONE',  ( -40.00000000000000000, 20.00000000000000000, 30.00000000000000355 ) ) ;
#8584 = DIRECTION ( 'NONE',  ( 0.000000000000000000, -0.000000000000000000, 1.000000000000000000 ) ) ;
#8585 = EDGE_CURVE ( 'NONE', #11464, #10357, #10844, .T. ) ;
#8586 = ORIENTED_EDGE ( 'NONE', *, *, #16428, .T. ) ;
#8587 = CARTESIAN_POINT ( 'NONE',  ( 32.50000000000000711, 146.6227766016838245, 1.387778780781445676E-14 ) ) ;
#8588 = CARTESIAN_POINT ( 'NONE',  ( -102.0000000000000142, 171.6227766016838245, 0.000000000000000000 ) ) ;
#8589 = ORIENTED_EDGE ( 'NONE', *, *, #14106, .F. ) ;
#8590 = CARTESIAN_POINT ( 'NONE',  ( 23.02032457293857348, 149.4008433394087092, -24.40281628369250200 ) ) ;
#8591 =( BOUNDED_SURFACE ( )  B_SPLINE_SURFACE ( 3, 2, ( 
 ( #16618, #13959, #1822 ),
 ( #4488, #14454, #16524 ),
 ( #12620, #16789, #9044 ),
 ( #8465, #11294, #12536 ),
 ( #13881, #14050, #7053 ),
 ( #9875, #3334, #7136 ),
 ( #4577, #6299, #401 ),
 ( #12454, #1910, #9958 ),
 ( #15282, #7308, #12715 ),
 ( #3155, #591, #5989 ),
 ( #8954, #14363, #2320 ),
 ( #6755, #6483, #14626 ),
 ( #1172, #2499, #2402 ),
 ( #16144, #6573, #13476 ),
 ( #7897, #13305, #15867 ),
 ( #6387, #10731, #3923 ),
 ( #9397, #11877, #11964 ),
 ( #5425, #7798, #15949 ),
 ( #2596, #12152, #10815 ),
 ( #5154, #22, #13119 ),
 ( #9472, #13210, #4018 ),
 ( #983, #14800, #6660 ),
 ( #17366, #4094, #17282 ),
 ( #14721, #11783, #16226 ),
 ( #1080, #3826, #5237 ),
 ( #12055, #17190, #7711 ),
 ( #10543, #9218, #9127 ),
 ( #5066, #9310, #10639 ),
 ( #16046, #7983, #2672 ),
 ( #8062, #13384, #1252 ) ),
 .UNSPECIFIED., .F., .F., .F. ) 
 B_SPLINE_SURFACE_WITH_KNOTS ( ( 4, 2, 2, 2, 2, 2, 2, 2, 2, 2, 2, 2, 2, 2, 4 ),
 ( 3, 3 ),
 ( 0.01165250788892075590, 0.01579789672993321681, 0.01787059115043944726, 0.01890693836069256423, 0.01994328557094567772, 0.02408867441195813863, 0.02616136883246436562, 0.02823406325297059608, 0.03030675767347682653, 0.03237945209398305352, 0.03652484093499551443, 0.03859753535550174142, 0.03963388256575485491, 0.04067022977600797534, 0.04481561861702043625 ),
 ( 0.000000000000000000, 1.000000000000000000 ),
 .UNSPECIFIED. ) 
 GEOMETRIC_REPRESENTATION_ITEM ( )  RATIONAL_B_SPLINE_SURFACE ( (
 ( 1.000000000000000000, 0.8819171036881968684, 1.000000000000000000),
 ( 1.000000000000000000, 0.8793942645247271317, 1.000000000000000000),
 ( 1.000000000000000000, 0.8749458316895473153, 1.000000000000000000),
 ( 1.000000000000000000, 0.8656814021268807169, 1.000000000000000000),
 ( 1.000000000000000000, 0.8621600075895787807, 1.000000000000000000),
 ( 1.000000000000000000, 0.8562492930711512740, 1.000000000000000000),
 ( 1.000000000000000000, 0.8541736901086096623, 1.000000000000000000),
 ( 1.000000000000000000, 0.8498659178638878764, 1.000000000000000000),
 ( 1.000000000000000000, 0.8476283308600994770, 1.000000000000000000),
 ( 1.000000000000000000, 0.8360458749413697266, 1.000000000000000000),
 ( 1.000000000000000000, 0.8255221978283152628, 1.000000000000000000),
 ( 1.000000000000000000, 0.8082270345000643896, 1.000000000000000000),
 ( 1.000000000000000000, 0.8022128341713220534, 1.000000000000000000),
 ( 1.000000000000000000, 0.7899684886175323273, 1.000000000000000000),
 ( 1.000000000000000000, 0.7837128169312477244, 1.000000000000000000),
 ( 1.000000000000000000, 0.7710263478628327505, 1.000000000000000000),
 ( 1.000000000000000000, 0.7645952338537677084, 1.000000000000000000),
 ( 1.000000000000000000, 0.7516613202047349729, 1.000000000000000000),
 ( 1.000000000000000000, 0.7451386183435962929, 1.000000000000000000),
 ( 1.000000000000000000, 0.7257808243687768890, 1.000000000000000000),
 ( 1.000000000000000000, 0.7133953845776382918, 1.000000000000000000),
 ( 1.000000000000000000, 0.6965170042221158209, 1.000000000000000000),
 ( 1.000000000000000000, 0.6911767420096451842, 1.000000000000000000),
 ( 1.000000000000000000, 0.6837405640632109316, 1.000000000000000000),
 ( 1.000000000000000000, 0.6813577907324296357, 1.000000000000000000),
 ( 1.000000000000000000, 0.6768117804540668692, 1.000000000000000000),
 ( 1.000000000000000000, 0.6746439590912666207, 1.000000000000000000),
 ( 1.000000000000000000, 0.6645663254999827352, 1.000000000000000000),
 ( 1.000000000000000000, 0.6588263891900785207, 1.000000000000000000),
 ( 1.000000000000000000, 0.6558243695371216431, 1.000000000000000000) ) ) 
 REPRESENTATION_ITEM ( '' )  SURFACE ( )  );
#8592 = CARTESIAN_POINT ( 'NONE',  ( -8.719536044788691598, 18.00000000000000711, 25.00000000000000000 ) ) ;
#8593 = DIRECTION ( 'NONE',  ( 0.000000000000000000, -1.000000000000000000, 6.123233995736762338E-17 ) ) ;
#8594 = CIRCLE ( 'NONE', #8865, 1.000000000000000888 ) ;
#8595 = DIRECTION ( 'NONE',  ( 0.000000000000000000, 0.000000000000000000, 1.000000000000000000 ) ) ;
#8596 = CARTESIAN_POINT ( 'NONE',  ( 0.000000000000000000, 18.00000000000000355, 0.000000000000000000 ) ) ;
#8597 = CIRCLE ( 'NONE', #2101, 20.00000000000000355 ) ;
#8598 = LINE ( 'NONE', #369, #971 ) ;
#8599 = CARTESIAN_POINT ( 'NONE',  ( -73.58001751434005655, 142.7179894756439751, -15.94334347237690430 ) ) ;
#8600 = VERTEX_POINT ( 'NONE', #9510 ) ;
#8601 = DIRECTION ( 'NONE',  ( 0.000000000000000000, 0.000000000000000000, 1.000000000000000000 ) ) ;
#8602 = ORIENTED_EDGE ( 'NONE', *, *, #2237, .T. ) ;
#8603 = DIRECTION ( 'NONE',  ( -6.938893903907228378E-16, 1.000000000000000000, 0.000000000000000000 ) ) ;
#8604 = ADVANCED_FACE ( 'NONE', ( #9254 ), #13338, .F. ) ;
#8605 = CARTESIAN_POINT ( 'NONE',  ( -116.4755503550297107, 171.6227766016838245, -78.75916623668499028 ) ) ;
#8606 = EDGE_CURVE ( 'NONE', #9042, #5256, #7373, .T. ) ;
#8607 = EDGE_CURVE ( 'NONE', #6756, #10807, #13016, .T. ) ;
#8608 = VERTEX_POINT ( 'NONE', #12263 ) ;
#8609 = CARTESIAN_POINT ( 'NONE',  ( -22.99999999999998224, 10.00000000000000000, -35.00200000000000244 ) ) ;
#8610 = CIRCLE ( 'NONE', #14547, 2.499999999999998668 ) ;
#8611 =( GEOMETRIC_REPRESENTATION_CONTEXT ( 3 ) GLOBAL_UNCERTAINTY_ASSIGNED_CONTEXT ( ( #14650 ) ) GLOBAL_UNIT_ASSIGNED_CONTEXT ( ( #12300, #14873, #3914 ) ) REPRESENTATION_CONTEXT ( 'NONE', 'WORKASPACE' ) );
#8612 = CARTESIAN_POINT ( 'NONE',  ( 27.48361012695778882, 136.6227766016838530, 1.300194169143111589 ) ) ;
#8613 = CARTESIAN_POINT ( 'NONE',  ( 16.31902522550215551, 136.8400131045044930, 5.103539400524462977 ) ) ;
#8614 = ORIENTED_EDGE ( 'NONE', *, *, #1484, .F. ) ;
#8615 = CARTESIAN_POINT ( 'NONE',  ( 27.99999999999998224, 9.999999999999998224, -16.00000000000000000 ) ) ;
#8616 = DIRECTION ( 'NONE',  ( -1.000000000000000000, -0.000000000000000000, -0.000000000000000000 ) ) ;
#8617 = DIRECTION ( 'NONE',  ( -1.000000000000000000, 0.000000000000000000, 0.000000000000000000 ) ) ;
#8618 = CARTESIAN_POINT ( 'NONE',  ( -100.0000000000000000, 142.5209969267753820, 19.44444444444445352 ) ) ;
#8619 = CARTESIAN_POINT ( 'NONE',  ( 15.45427063382542165, 18.00000000000226663, 13.01057400152831711 ) ) ;
#8620 = CARTESIAN_POINT ( 'NONE',  ( 25.00000000000000711, 146.6227766016838245, 0.000000000000000000 ) ) ;
#8621 = AXIS2_PLACEMENT_3D ( 'NONE', #8423, #13841, #8595 ) ;
#8622 = ORIENTED_EDGE ( 'NONE', *, *, #5852, .F. ) ;
#8623 = CARTESIAN_POINT ( 'NONE',  ( -68.00000000000000000, 154.3022685259950038, -9.999999999999900524 ) ) ;
#8625 = DIRECTION ( 'NONE',  ( 1.000000000000000000, 0.000000000000000000, 0.000000000000000000 ) ) ;
#8624 = CIRCLE ( 'NONE', #13721, 30.00000000000000000 ) ;
#8626 = ORIENTED_EDGE ( 'NONE', *, *, #15550, .F. ) ;
#8627 = FACE_OUTER_BOUND ( 'NONE', #16322, .T. ) ;
#8628 = PLANE ( 'NONE',  #4702 ) ;
#8629 = EDGE_CURVE ( 'NONE', #15706, #7981, #13515, .T. ) ;
#8630 = ORIENTED_EDGE ( 'NONE', *, *, #2005, .T. ) ;
#8631 = ADVANCED_FACE ( 'NONE', ( #6696 ), #14724, .T. ) ;
#8632 = ORIENTED_EDGE ( 'NONE', *, *, #1653, .F. ) ;
#8633 = ORIENTED_EDGE ( 'NONE', *, *, #17303, .T. ) ;
#8634 = CARTESIAN_POINT ( 'NONE',  ( 1.559999999999998943, 0.8660254037844428154, 1.500000000000001332 ) ) ;
#8635 = ORIENTED_EDGE ( 'NONE', *, *, #4377, .T. ) ;
#8636 = CARTESIAN_POINT ( 'NONE',  ( -187.6513770290094953, 169.2829632032627956, -0.3407269638998823291 ) ) ;
#8637 = B_SPLINE_CURVE_WITH_KNOTS ( 'NONE', 3,
 ( #8536, #12440, #4381, #7124 ),
 .UNSPECIFIED., .F., .F.,
 ( 4, 4 ),
 ( 0.000000000000000000, 0.005007666328367723664 ),
 .UNSPECIFIED. ) ;
#8638 = MECHANICAL_DESIGN_GEOMETRIC_PRESENTATION_REPRESENTATION (  '', ( #3546 ), #10614 ) ;
#8639 = ORIENTED_EDGE ( 'NONE', *, *, #7097, .F. ) ;
#8640 = FILL_AREA_STYLE ('',( #1914 ) ) ;
#8641 = DIRECTION ( 'NONE',  ( -1.000000000000000000, -0.000000000000000000, -0.000000000000000000 ) ) ;
#8642 = CIRCLE ( 'NONE', #16844, 750.0000000000000000 ) ;
#8643 = CIRCLE ( 'NONE', #1001, 10.00000000000000178 ) ;
#8644 = DIRECTION ( 'NONE',  ( 0.000000000000000000, 1.000000000000000000, 0.000000000000000000 ) ) ;
#8645 = DIRECTION ( 'NONE',  ( 0.000000000000000000, 0.000000000000000000, -1.000000000000000000 ) ) ;
#8646 = DIRECTION ( 'NONE',  ( -1.000000000000000000, 0.000000000000000000, 0.000000000000000000 ) ) ;
#8647 = ORIENTED_EDGE ( 'NONE', *, *, #16200, .F. ) ;
#8648 = CARTESIAN_POINT ( 'NONE',  ( 29.75497873520074421, 141.6230733471410304, 13.74837463607936883 ) ) ;
#8649 = CARTESIAN_POINT ( 'NONE',  ( -50.00000000000000711, -20.00000000000000000, 40.00000000000000711 ) ) ;
#8650 = DIRECTION ( 'NONE',  ( 0.000000000000000000, 0.000000000000000000, -1.000000000000000000 ) ) ;
#8651 = B_SPLINE_CURVE_WITH_KNOTS ( 'NONE', 3,
 ( #10476, #10554, #7557, #841, #14642, #2514, #13319, #11544, #12966, #13400, #8078, #16330 ),
 .UNSPECIFIED., .F., .F.,
 ( 4, 2, 2, 2, 2, 4 ),
 ( 0.000000000000000000, 0.0006954760458707579234, 0.001390952091741515847, 0.001738690114676866294, 0.002086428137612216741, 0.002781904183482844344 ),
 .UNSPECIFIED. ) ;
#8652 = EDGE_CURVE ( 'NONE', #1245, #11878, #15277, .T. ) ;
#8653 = CARTESIAN_POINT ( 'NONE',  ( -12.78554710720352894, 31.18907022382790117, -13.71297843187037202 ) ) ;
#8654 = CYLINDRICAL_SURFACE ( 'NONE', #9772, 3.999999999999988010 ) ;
#8655 = AXIS2_PLACEMENT_3D ( 'NONE', #2780, #12428, #4288 ) ;
#8656 = B_SPLINE_CURVE_WITH_KNOTS ( 'NONE', 3,
 ( #10991, #13576, #14806, #8249 ),
 .UNSPECIFIED., .F., .F.,
 ( 4, 4 ),
 ( 0.000000000000000000, 0.005007666328367723664 ),
 .UNSPECIFIED. ) ;
#8657 = AXIS2_PLACEMENT_3D ( 'NONE', #3752, #17205, #2419 ) ;
#8658 = CYLINDRICAL_SURFACE ( 'NONE', #15826, 2.500000000000002220 ) ;
#8659 = EDGE_LOOP ( 'NONE', ( #4458, #9821 ) ) ;
#8660 = LINE ( 'NONE', #5924, #12346 ) ;
#8661 = EDGE_LOOP ( 'NONE', ( #15110, #16420, #3102, #5987, #3998 ) ) ;
#8662 = CARTESIAN_POINT ( 'NONE',  ( 25.83188736168996513, 137.9746650487458908, 9.688332914129558660 ) ) ;
#8664 = VERTEX_POINT ( 'NONE', #8274 ) ;
#8663 = AXIS2_PLACEMENT_3D ( 'NONE', #2495, #3650, #2593 ) ;
#8665 = AXIS2_PLACEMENT_3D ( 'NONE', #193, #2769, #2932 ) ;
#8666 = CARTESIAN_POINT ( 'NONE',  ( 15.00000000000000000, 171.6227766016838245, 0.000000000000000000 ) ) ;
#8667 = AXIS2_PLACEMENT_3D ( 'NONE', #6734, #6642, #2581 ) ;
#8668 = DIRECTION ( 'NONE',  ( 1.000000000000000000, -0.000000000000000000, -0.000000000000000000 ) ) ;
#8669 = VERTEX_POINT ( 'NONE', #12444 ) ;
#8670 = DIRECTION ( 'NONE',  ( 0.000000000000000000, 0.000000000000000000, 1.000000000000000000 ) ) ;
#8671 = PLANE ( 'NONE',  #10137 ) ;
#8672 = CARTESIAN_POINT ( 'NONE',  ( 21.99999999999998224, 9.999999999999998224, -16.00000000000000000 ) ) ;
#8673 = EDGE_CURVE ( 'NONE', #3629, #6874, #5969, .T. ) ;
#8674 = PLANE ( 'NONE',  #9758 ) ;
#8675 = ORIENTED_EDGE ( 'NONE', *, *, #12801, .T. ) ;
#8676 = ORIENTED_EDGE ( 'NONE', *, *, #1454, .T. ) ;
#8677 = CARTESIAN_POINT ( 'NONE',  ( 32.90650748920315039, 19.99999999999999645, -13.87185692902932921 ) ) ;
#8678 = VECTOR ( 'NONE', #5048, 1000.000000000000000 ) ;
#8679 = CARTESIAN_POINT ( 'NONE',  ( 21.47128797932978372, 141.5899928260317040, -13.68519783011616653 ) ) ;
#8680 = CIRCLE ( 'NONE', #16885, 2.499999999999999112 ) ;
#8681 = VERTEX_POINT ( 'NONE', #11285 ) ;
#8682 = ADVANCED_FACE ( 'NONE', ( #316 ), #4389, .F. ) ;
#8683 = DIRECTION ( 'NONE',  ( -1.000000000000000000, 0.000000000000000000, -8.673617379884037937E-17 ) ) ;
#8684 = ADVANCED_FACE ( 'NONE', ( #8456 ), #15084, .T. ) ;
#8685 = PRESENTATION_LAYER_ASSIGNMENT (  '', '', ( #1620 ) ) ;
#8686 = DIRECTION ( 'NONE',  ( -1.000000000000000000, 0.000000000000000000, 0.000000000000000000 ) ) ;
#8687 = EDGE_LOOP ( 'NONE', ( #5106, #10512, #563, #4610 ) ) ;
#8688 = CARTESIAN_POINT ( 'NONE',  ( 35.27494917608787972, 201.9542783778900059, -13.00000000000000000 ) ) ;
#8689 = CARTESIAN_POINT ( 'NONE',  ( -26.10410744458347665, 18.00000000000000000, 13.37721135299797304 ) ) ;
#8690 = CARTESIAN_POINT ( 'NONE',  ( -43.00000000000000711, 130.0000000000000000, 12.99999999999999822 ) ) ;
#8691 = CARTESIAN_POINT ( 'NONE',  ( -206.6025269363104826, 174.5791181652666353, 3.990821701952568468 ) ) ;
#8692 = DIRECTION ( 'NONE',  ( 0.000000000000000000, 0.000000000000000000, 1.000000000000000000 ) ) ;
#8693 = CONICAL_SURFACE ( 'NONE', #8972, 35.00000000000000000, 0.5235987755983005920 ) ;
#8694 = DIRECTION ( 'NONE',  ( -1.000000000000000000, -0.000000000000000000, -0.000000000000000000 ) ) ;
#8695 = AXIS2_PLACEMENT_3D ( 'NONE', #6708, #13522, #13789 ) ;
#8696 = DIRECTION ( 'NONE',  ( 1.000000000000000000, 1.156482317317868274E-16, 0.000000000000000000 ) ) ;
#8697 = EDGE_LOOP ( 'NONE', ( #5777, #4613, #16496, #4846 ) ) ;
#8698 = DIRECTION ( 'NONE',  ( 0.000000000000000000, 0.000000000000000000, 1.000000000000000000 ) ) ;
#8699 = ORIENTED_EDGE ( 'NONE', *, *, #843, .T. ) ;
#8700 = DIRECTION ( 'NONE',  ( -1.000000000000000000, -0.000000000000000000, 0.000000000000000000 ) ) ;
#8701 = DIRECTION ( 'NONE',  ( -0.000000000000000000, -0.000000000000000000, 1.000000000000000000 ) ) ;
#8702 = ORIENTED_EDGE ( 'NONE', *, *, #364, .T. ) ;
#8703 = DIRECTION ( 'NONE',  ( 0.9961946980917461003, -0.04357787137382522491, -0.07547908730516825204 ) ) ;
#8704 =( BOUNDED_CURVE ( )  B_SPLINE_CURVE ( 3, ( #9180, #17331, #3886, #14679 ),
 .UNSPECIFIED., .F., .F. ) 
 B_SPLINE_CURVE_WITH_KNOTS ( ( 4, 4 ),
 ( 4.792629041327348460, 6.283185307179586232 ),
 .UNSPECIFIED. ) 
 CURVE ( )  GEOMETRIC_REPRESENTATION_ITEM ( )  RATIONAL_B_SPLINE_CURVE ( ( 1.000000000000000000, 0.8232662051119113977, 0.8232662051119113977, 1.000000000000000000 ) ) 
 REPRESENTATION_ITEM ( '' )  );
#8705 = AXIS2_PLACEMENT_3D ( 'NONE', #14038, #12706, #7207 ) ;
#8706 = CARTESIAN_POINT ( 'NONE',  ( 24.60025152864608700, 29.87271304632927027, 7.586598161752979408 ) ) ;
#8707 = CARTESIAN_POINT ( 'NONE',  ( 26.57417986947462651, 137.5626638350942699, 8.060801806284990434 ) ) ;
#8708 = CIRCLE ( 'NONE', #2192, 2.499999999999998668 ) ;
#8709 = ORIENTED_EDGE ( 'NONE', *, *, #6612, .T. ) ;
#8710 = DIRECTION ( 'NONE',  ( -1.000000000000000000, -0.000000000000000000, -0.000000000000000000 ) ) ;
#8711 = CARTESIAN_POINT ( 'NONE',  ( -5.000000000000000888, 154.3022685259950038, -9.999999999999900524 ) ) ;
#8712 = CARTESIAN_POINT ( 'NONE',  ( -77.12399049755265423, 192.5178712342568303, 25.54362227291155207 ) ) ;
#8713 = CARTESIAN_POINT ( 'NONE',  ( 27.44407568426044364, 136.8394969516870958, -3.888888888888887063 ) ) ;
#8714 = EDGE_CURVE ( 'NONE', #11591, #8346, #15290, .T. ) ;
#8715 = CARTESIAN_POINT ( 'NONE',  ( 19.14963388379466736, 18.00000000000000000, 24.55317681541934149 ) ) ;
#8716 = PRODUCT ( 'Keyless Chuck', 'Keyless Chuck', '', ( #16340 ) ) ;
#8717 = CARTESIAN_POINT ( 'NONE',  ( 27.30499999999999616, 3.061616997868382648E-16, -2.499999999999999556 ) ) ;
#8718 = VERTEX_POINT ( 'NONE', #5631 ) ;
#8719 = DIRECTION ( 'NONE',  ( -1.000000000000000000, 0.000000000000000000, 0.000000000000000000 ) ) ;
#8720 = AXIS2_PLACEMENT_3D ( 'NONE', #11102, #4387, #9776 ) ;
#8721 = CARTESIAN_POINT ( 'NONE',  ( 196.0000000000000000, 187.6227766016837961, -10.00000337241049309 ) ) ;
#8722 = ORIENTED_EDGE ( 'NONE', *, *, #6232, .T. ) ;
#8723 = LINE ( 'NONE', #15181, #7329 ) ;
#8724 = AXIS2_PLACEMENT_3D ( 'NONE', #16126, #9113, #10799 ) ;
#8725 = FACE_BOUND ( 'NONE', #7112, .T. ) ;
#8726 = ORIENTED_EDGE ( 'NONE', *, *, #14951, .T. ) ;
#8727 = ORIENTED_EDGE ( 'NONE', *, *, #7281, .T. ) ;
#8728 = ORIENTED_EDGE ( 'NONE', *, *, #7317, .F. ) ;
#8729 = ORIENTED_EDGE ( 'NONE', *, *, #8714, .F. ) ;
#8730 = DIRECTION ( 'NONE',  ( -0.000000000000000000, -0.000000000000000000, -1.000000000000000000 ) ) ;
#8731 = VERTEX_POINT ( 'NONE', #1552 ) ;
#8732 = VECTOR ( 'NONE', #1022, 1000.000000000000000 ) ;
#8733 = CARTESIAN_POINT ( 'NONE',  ( 196.0000000000000000, 175.6227766016838245, -3.071800142134975431 ) ) ;
#8734 = CIRCLE ( 'NONE', #14658, 2.055000000000000160 ) ;
#8735 = DIRECTION ( 'NONE',  ( 0.000000000000000000, 0.000000000000000000, -1.000000000000000000 ) ) ;
#8736 = EDGE_CURVE ( 'NONE', #1044, #15578, #873, .T. ) ;
#8737 = EDGE_CURVE ( 'NONE', #5595, #11327, #1904, .T. ) ;
#8738 = CARTESIAN_POINT ( 'NONE',  ( -15.00000000000002487, 120.0000000000000284, -4.999999999999999112 ) ) ;
#8739 = EDGE_CURVE ( 'NONE', #7262, #9320, #14175, .T. ) ;
#8740 = VERTEX_POINT ( 'NONE', #482 ) ;
#8741 = DIRECTION ( 'NONE',  ( 0.000000000000000000, 1.000000000000000000, 0.000000000000000000 ) ) ;
#8742 = CARTESIAN_POINT ( 'NONE',  ( -80.00000000000002842, 146.6227766016838245, 0.000000000000000000 ) ) ;
#8743 = CARTESIAN_POINT ( 'NONE',  ( -33.99999999999997868, 10.00000000000000000, -35.00000000000000000 ) ) ;
#8744 = CARTESIAN_POINT ( 'NONE',  ( -13.95500183466744382, 31.43484250012364001, -12.98634364776042638 ) ) ;
#8745 = CIRCLE ( 'NONE', #5060, 2.499999999999998668 ) ;
#8746 = AXIS2_PLACEMENT_3D ( 'NONE', #3208, #16841, #12425 ) ;
#8747 = VECTOR ( 'NONE', #4753, 1000.000000000000000 ) ;
#8748 = DIRECTION ( 'NONE',  ( -0.000000000000000000, -0.000000000000000000, -1.000000000000000000 ) ) ;
#8749 = ORIENTED_EDGE ( 'NONE', *, *, #6232, .F. ) ;
#8750 = CARTESIAN_POINT ( 'NONE',  ( 27.44407568426044364, 136.8394969516870958, -3.888888888888887063 ) ) ;
#8751 = ORIENTED_EDGE ( 'NONE', *, *, #16101, .F. ) ;
#8752 = CARTESIAN_POINT ( 'NONE',  ( 10.42241938378121624, 142.2974014187406055, 19.10582184898306224 ) ) ;
#8753 = DIRECTION ( 'NONE',  ( -0.000000000000000000, -0.000000000000000000, 1.000000000000000000 ) ) ;
#8754 = VECTOR ( 'NONE', #13626, 1000.000000000000000 ) ;
#8755 = AXIS2_PLACEMENT_3D ( 'NONE', #9172, #11828, #10585 ) ;
#8756 = CYLINDRICAL_SURFACE ( 'NONE', #16521, 2.500000000000000444 ) ;
#8757 = ORIENTED_EDGE ( 'NONE', *, *, #16378, .T. ) ;
#8758 = DIRECTION ( 'NONE',  ( 0.000000000000000000, 0.000000000000000000, -1.000000000000000000 ) ) ;
#8759 = CARTESIAN_POINT ( 'NONE',  ( 0.000000000000000000, 0.000000000000000000, 0.000000000000000000 ) ) ;
#8760 = CARTESIAN_POINT ( 'NONE',  ( -80.60934097988227620, 201.5868197762109162, 13.82597759728682796 ) ) ;
#8761 = CARTESIAN_POINT ( 'NONE',  ( 31.78129305203702870, 202.3573166656175033, -16.74530232247016315 ) ) ;
#8762 = ORIENTED_EDGE ( 'NONE', *, *, #15065, .F. ) ;
#8763 = ORIENTED_EDGE ( 'NONE', *, *, #2875, .T. ) ;
#8764 = CARTESIAN_POINT ( 'NONE',  ( 14.93242934743711814, 30.00000000000000000, -15.00000000000000000 ) ) ;
#8765 = AXIS2_PLACEMENT_3D ( 'NONE', #3175, #13975, #5824 ) ;
#8766 = AXIS2_PLACEMENT_3D ( 'NONE', #11587, #15651, #7682 ) ;
#8767 = CARTESIAN_POINT ( 'NONE',  ( -71.66708739526794147, 110.0000000000000142, 5.500000000000000000 ) ) ;
#8768 = VERTEX_POINT ( 'NONE', #15273 ) ;
#8769 = DIRECTION ( 'NONE',  ( -1.000000000000000000, 0.000000000000000000, 0.000000000000000000 ) ) ;
#8770 = AXIS2_PLACEMENT_3D ( 'NONE', #11763, #10439, #16208 ) ;
#8771 = CARTESIAN_POINT ( 'NONE',  ( 9.072488053085830728, 140.2836875516620978, -12.31648485192419784 ) ) ;
#8772 = ORIENTED_EDGE ( 'NONE', *, *, #15327, .T. ) ;
#8773 = EDGE_CURVE ( 'NONE', #13751, #9170, #315, .T. ) ;
#8774 = DIRECTION ( 'NONE',  ( 8.673617379884037937E-17, 0.000000000000000000, -1.000000000000000000 ) ) ;
#8775 = UNCERTAINTY_MEASURE_WITH_UNIT (LENGTH_MEASURE( 1.000000000000000082E-05 ), #148, 'distance_accuracy_value', 'NONE');
#8776 = ADVANCED_FACE ( 'NONE', ( #16517 ), #6239, .F. ) ;
#8777 = PLANE ( 'NONE',  #2162 ) ;
#8778 = CARTESIAN_POINT ( 'NONE',  ( 30.00000000000001066, 146.6227766016838245, 0.000000000000000000 ) ) ;
#8779 = VECTOR ( 'NONE', #16257, 1000.000000000000000 ) ;
#8780 = CARTESIAN_POINT ( 'NONE',  ( -12.80328004468388770, 17.99999999999770850, 5.290760321145405953 ) ) ;
#8781 = CARTESIAN_POINT ( 'NONE',  ( -22.93725393319378369, 20.00000000000004263, -5.999999999999992895 ) ) ;
#8782 = AXIS2_PLACEMENT_3D ( 'NONE', #11095, #16341, #4209 ) ;
#8783 = ADVANCED_FACE ( 'NONE', ( #13951 ), #15179, .T. ) ;
#8784 = CARTESIAN_POINT ( 'NONE',  ( 30.27573706856752622, 140.6276388071887595, -16.25736180127249852 ) ) ;
#8785 = ORIENTED_EDGE ( 'NONE', *, *, #9166, .F. ) ;
#8786 = CARTESIAN_POINT ( 'NONE',  ( 1.559999999999998943, 1.732050807568885631, 0.000000000000000000 ) ) ;
#8787 = EDGE_LOOP ( 'NONE', ( #10884, #6890 ) ) ;
#8788 = CARTESIAN_POINT ( 'NONE',  ( -197.9999999999999716, 171.6227766016838245, 0.000000000000000000 ) ) ;
#8789 = CARTESIAN_POINT ( 'NONE',  ( -68.00000000000000000, 204.6227766016838245, 0.000000000000000000 ) ) ;
#8790 = VERTEX_POINT ( 'NONE', #3051 ) ;
#8791 = DIRECTION ( 'NONE',  ( 1.000000000000000000, 0.000000000000000000, 0.000000000000000000 ) ) ;
#8792 = CIRCLE ( 'NONE', #1157, 2.500000000000000000 ) ;
#8793 = CARTESIAN_POINT ( 'NONE',  ( 23.77503517897789465, 19.99999999999999645, 22.95135521423388170 ) ) ;
#8794 = CARTESIAN_POINT ( 'NONE',  ( 26.46962346220079709, 137.6228726052619606, 8.310907492956932430 ) ) ;
#8795 = EDGE_CURVE ( 'NONE', #15177, #1173, #12186, .T. ) ;
#8796 = VERTEX_POINT ( 'NONE', #4481 ) ;
#8797 = DIRECTION ( 'NONE',  ( 0.000000000000000000, 0.9938079899999066047, -0.1111111111111111188 ) ) ;
#8798 = CARTESIAN_POINT ( 'NONE',  ( -80.97044773050417632, 191.7140209832037954, 26.17909706909632561 ) ) ;
#8799 = EDGE_CURVE ( 'NONE', #9221, #8198, #9866, .T. ) ;
#8800 = CARTESIAN_POINT ( 'NONE',  ( -18.25212770525997286, 32.30769230769230660, -4.999999999999999112 ) ) ;
#8801 = CARTESIAN_POINT ( 'NONE',  ( -85.00000000000002842, 146.6227766016838245, 35.00200000000000244 ) ) ;
#8802 = DIRECTION ( 'NONE',  ( 0.000000000000000000, 0.000000000000000000, -1.000000000000000000 ) ) ;
#8803 = EDGE_CURVE ( 'NONE', #13322, #10334, #5889, .T. ) ;
#8804 = ADVANCED_FACE ( 'NONE', ( #9952 ), #7300, .F. ) ;
#8805 = ORIENTED_EDGE ( 'NONE', *, *, #1544, .F. ) ;
#8806 = CARTESIAN_POINT ( 'NONE',  ( 30.00000000000000355, 196.6227766016838245, -35.00200000000000244 ) ) ;
#8807 = CIRCLE ( 'NONE', #2864, 12.00000000000000000 ) ;
#8808 = CARTESIAN_POINT ( 'NONE',  ( -18.25212770525996930, 32.30769230769230660, 0.000000000000000000 ) ) ;
#8809 = VERTEX_POINT ( 'NONE', #4647 ) ;
#8810 = FACE_OUTER_BOUND ( 'NONE', #2708, .T. ) ;
#8811 = CARTESIAN_POINT ( 'NONE',  ( 225.0000000000000000, 89.99999999999997158, 0.000000000000000000 ) ) ;
#8812 = VERTEX_POINT ( 'NONE', #8808 ) ;
#8813 = VERTEX_POINT ( 'NONE', #14286 ) ;
#8814 = ADVANCED_FACE ( 'NONE', ( #16956 ), #12964, .F. ) ;
#8815 = ORIENTED_EDGE ( 'NONE', *, *, #13705, .T. ) ;
#8816 = DIRECTION ( 'NONE',  ( -0.000000000000000000, -0.000000000000000000, -1.000000000000000000 ) ) ;
#8817 = VERTEX_POINT ( 'NONE', #10126 ) ;
#8818 = CARTESIAN_POINT ( 'NONE',  ( 196.0000000000000000, 191.6227766016837677, 8.071800142134975431 ) ) ;
#8819 = DIRECTION ( 'NONE',  ( -0.000000000000000000, -0.000000000000000000, -1.000000000000000000 ) ) ;
#8820 = VERTEX_POINT ( 'NONE', #6058 ) ;
#8821 = CARTESIAN_POINT ( 'NONE',  ( -22.99999999999999289, 90.00000000000000000, -4.999999999999999112 ) ) ;
#8822 = DIRECTION ( 'NONE',  ( -3.469446951953613696E-16, 1.000000000000000000, -0.000000000000000000 ) ) ;
#8823 = DIRECTION ( 'NONE',  ( -1.000000000000000000, 0.000000000000000000, 0.000000000000000000 ) ) ;
#8824 = CARTESIAN_POINT ( 'NONE',  ( -9.703671380219324405, 20.00000000000114397, -14.18606485937966788 ) ) ;
#8825 = CARTESIAN_POINT ( 'NONE',  ( -23.00000000000000000, 120.0000000000000284, 15.00000000000000000 ) ) ;
#8826 = CARTESIAN_POINT ( 'NONE',  ( -168.0000000000000284, 168.3180863238818006, -5.723891464432168341 ) ) ;
#8827 = EDGE_CURVE ( 'NONE', #2297, #233, #5113, .T. ) ;
#8828 = EDGE_CURVE ( 'NONE', #3065, #4370, #3324, .T. ) ;
#8829 = EDGE_CURVE ( 'NONE', #15643, #11995, #15405, .T. ) ;
#8830 = ORIENTED_EDGE ( 'NONE', *, *, #13216, .F. ) ;
#8831 = CYLINDRICAL_SURFACE ( 'NONE', #4443, 2.500000000000002220 ) ;
#8832 = ORIENTED_EDGE ( 'NONE', *, *, #6071, .F. ) ;
#8833 = APPLICATION_PROTOCOL_DEFINITION ( 'draft international standard', 'automotive_design', 1998, #4939 ) ;
#8834 = DIRECTION ( 'NONE',  ( -1.000000000000000000, -0.000000000000000000, -0.000000000000000000 ) ) ;
#8835 = CARTESIAN_POINT ( 'NONE',  ( -43.00000000000000000, 171.6227766016838245, 0.000000000000000000 ) ) ;
#8836 = DIRECTION ( 'NONE',  ( 0.8660254037844378194, -0.5000000000000015543, -0.000000000000000000 ) ) ;
#8837 = ORIENTED_EDGE ( 'NONE', *, *, #8412, .T. ) ;
#8838 = CARTESIAN_POINT ( 'NONE',  ( -2.428612866367531510E-15, 18.00000000000000355, -28.00000000000000711 ) ) ;
#8839 = PLANE ( 'NONE',  #7620 ) ;
#8840 = CARTESIAN_POINT ( 'NONE',  ( 31.31294070251087192, 202.4787130041031560, -16.52010876963832331 ) ) ;
#8841 = EDGE_LOOP ( 'NONE', ( #6766, #6868, #3575, #1254 ) ) ;
#8842 = ORIENTED_EDGE ( 'NONE', *, *, #16680, .F. ) ;
#8843 = CARTESIAN_POINT ( 'NONE',  ( 22.30340133326367180, 19.99999999999999645, -11.90876978475634651 ) ) ;
#8844 = DIRECTION ( 'NONE',  ( -1.000000000000000000, -0.000000000000000000, -0.000000000000000000 ) ) ;
#8845 = EDGE_CURVE ( 'NONE', #14384, #7220, #1444, .T. ) ;
#8846 = ORIENTED_EDGE ( 'NONE', *, *, #13706, .F. ) ;
#8847 = CARTESIAN_POINT ( 'NONE',  ( -15.00000000000002487, 120.0000000000000284, -4.999999999999999112 ) ) ;
#8848 = FACE_OUTER_BOUND ( 'NONE', #1143, .T. ) ;
#8849 = VERTEX_POINT ( 'NONE', #11628 ) ;
#8850 = DIRECTION ( 'NONE',  ( 0.000000000000000000, 0.000000000000000000, 1.000000000000000000 ) ) ;
#8851 = DIRECTION ( 'NONE',  ( 0.000000000000000000, 1.000000000000000000, 0.000000000000000000 ) ) ;
#8852 = CARTESIAN_POINT ( 'NONE',  ( 17.00000000000000000, 143.0439382767972631, 16.49999999999984013 ) ) ;
#8853 = CARTESIAN_POINT ( 'NONE',  ( -15.09627865792072576, 32.41573384469808161, 9.048329374498470301 ) ) ;
#8854 = DIRECTION ( 'NONE',  ( 1.000000000000000000, 0.000000000000000000, 0.000000000000000000 ) ) ;
#8855 = CYLINDRICAL_SURFACE ( 'NONE', #9447, 20.00000000000000355 ) ;
#8856 = EDGE_LOOP ( 'NONE', ( #10763, #3110 ) ) ;
#8857 = CARTESIAN_POINT ( 'NONE',  ( -27.98221281347037959, 30.00000000000000000, 15.00000000000000000 ) ) ;
#8858 = ORIENTED_EDGE ( 'NONE', *, *, #16392, .F. ) ;
#8859 = EDGE_CURVE ( 'NONE', #17193, #15663, #14211, .T. ) ;
#8860 = DIRECTION ( 'NONE',  ( -1.000000000000000000, 0.000000000000000000, 0.000000000000000000 ) ) ;
#8861 = CARTESIAN_POINT ( 'NONE',  ( -24.99999999999999645, 120.0000000000000284, -15.00000000000000000 ) ) ;
#8862 = ORIENTED_EDGE ( 'NONE', *, *, #15803, .F. ) ;
#8863 = FACE_OUTER_BOUND ( 'NONE', #17406, .T. ) ;
#8864 = CARTESIAN_POINT ( 'NONE',  ( -74.72505082391211317, 201.9542783778900059, -13.00000000000000000 ) ) ;
#8865 = AXIS2_PLACEMENT_3D ( 'NONE', #1849, #12481, #7250 ) ;
#8866 = ORIENTED_EDGE ( 'NONE', *, *, #9268, .T. ) ;
#8867 = FACE_OUTER_BOUND ( 'NONE', #6039, .T. ) ;
#8868 = CARTESIAN_POINT ( 'NONE',  ( -34.99999999999999289, 130.0000000000000000, -15.00000000000000000 ) ) ;
#8869 = DIRECTION ( 'NONE',  ( -1.000000000000000000, -0.000000000000000000, 0.000000000000000000 ) ) ;
#8870 = DIRECTION ( 'NONE',  ( 0.000000000000000000, 0.000000000000000000, 1.000000000000000000 ) ) ;
#8871 = PLANE ( 'NONE',  #6062 ) ;
#8872 = ORIENTED_EDGE ( 'NONE', *, *, #13599, .T. ) ;
#8873 = CARTESIAN_POINT ( 'NONE',  ( 30.00000000000001066, 146.6227766016838245, 0.000000000000000000 ) ) ;
#8874 = CARTESIAN_POINT ( 'NONE',  ( 30.00000000000001066, 146.6227766016838245, -35.00000000000000000 ) ) ;
#8875 = ORIENTED_EDGE ( 'NONE', *, *, #14562, .T. ) ;
#8876 = EDGE_CURVE ( 'NONE', #15136, #4720, #10204, .T. ) ;
#8877 = DIRECTION ( 'NONE',  ( 0.000000000000000000, 0.000000000000000000, -1.000000000000000000 ) ) ;
#8878 = LINE ( 'NONE', #17035, #7521 ) ;
#8879 = AXIS2_PLACEMENT_3D ( 'NONE', #2391, #16031, #7785 ) ;
#8880 = ORIENTED_EDGE ( 'NONE', *, *, #4303, .F. ) ;
#8881 = AXIS2_PLACEMENT_3D ( 'NONE', #10890, #1440, #12574 ) ;
#8882 = ORIENTED_EDGE ( 'NONE', *, *, #6876, .T. ) ;
#8883 = ORIENTED_EDGE ( 'NONE', *, *, #564, .F. ) ;
#8884 = EDGE_CURVE ( 'NONE', #11165, #12401, #16035, .T. ) ;
#8885 = ADVANCED_FACE ( 'NONE', ( #8419 ), #15324, .T. ) ;
#8886 = CARTESIAN_POINT ( 'NONE',  ( -87.50000000000002842, 146.8102797458443547, -21.75827460206394193 ) ) ;
#8887 = EDGE_CURVE ( 'NONE', #6145, #874, #1784, .T. ) ;
#8888 = ORIENTED_EDGE ( 'NONE', *, *, #9681, .F. ) ;
#8889 = LINE ( 'NONE', #766, #9620 ) ;
#8890 = LINE ( 'NONE', #14299, #9198 ) ;
#8891 = CONICAL_SURFACE ( 'NONE', #9756, 2.055000000000000160, 0.7853981633974428389 ) ;
#8892 = DIRECTION ( 'NONE',  ( 1.000000000000000000, -0.000000000000000000, -0.000000000000000000 ) ) ;
#8893 = CARTESIAN_POINT ( 'NONE',  ( 22.42543865150203075, 29.85191494357712116, 7.821916630904659939 ) ) ;
#8894 = DIRECTION ( 'NONE',  ( 1.000000000000000000, 0.000000000000000000, 0.000000000000000000 ) ) ;
#8895 = VECTOR ( 'NONE', #1201, 1000.000000000000000 ) ;
#8896 = VERTEX_POINT ( 'NONE', #16753 ) ;
#8897 = DIRECTION ( 'NONE',  ( -1.000000000000000000, 0.000000000000000000, 0.000000000000000000 ) ) ;
#8898 = CARTESIAN_POINT ( 'NONE',  ( 27.44407568426044008, 126.9014170516880284, -4.999999999999997335 ) ) ;
#8899 = DIRECTION ( 'NONE',  ( 0.000000000000000000, 0.000000000000000000, 1.000000000000000000 ) ) ;
#8900 = CARTESIAN_POINT ( 'NONE',  ( -3.000000000000000888, 191.6227766016837961, 1.224646799147353454E-15 ) ) ;
#8901 = CARTESIAN_POINT ( 'NONE',  ( -208.0000000000000853, 174.7326106162513497, 0.000000000000000000 ) ) ;
#8902 = VECTOR ( 'NONE', #5603, 1000.000000000000000 ) ;
#8903 = CARTESIAN_POINT ( 'NONE',  ( 33.42689610971938663, 200.2770367110203722, 16.37379161636572178 ) ) ;
#8904 = ORIENTED_EDGE ( 'NONE', *, *, #13025, .F. ) ;
#8905 = LINE ( 'NONE', #5826, #4729 ) ;
#8906 = AXIS2_PLACEMENT_3D ( 'NONE', #11144, #4343, #13995 ) ;
#8907 = CARTESIAN_POINT ( 'NONE',  ( -5.000000000000000888, 171.6227766016838245, 0.000000000000000000 ) ) ;
#8908 = ORIENTED_EDGE ( 'NONE', *, *, #11643, .T. ) ;
#8909 = PRODUCT_CONTEXT ( 'NONE', #10363, 'mechanical' ) ;
#8910 = DIRECTION ( 'NONE',  ( -0.000000000000000000, -0.000000000000000000, 1.000000000000000000 ) ) ;
#8911 = DIRECTION ( 'NONE',  ( 0.000000000000000000, 0.000000000000000000, -1.000000000000000000 ) ) ;
#8912 = DIRECTION ( 'NONE',  ( 0.9961946980917463224, -0.04357787137382344855, -0.07547908730516518505 ) ) ;
#8913 = VECTOR ( 'NONE', #10591, 1000.000000000000000 ) ;
#8914 = ORIENTED_EDGE ( 'NONE', *, *, #6341, .F. ) ;
#8915 = DIRECTION ( 'NONE',  ( -1.000000000000000000, 0.000000000000000000, 0.000000000000000000 ) ) ;
#8916 = DIRECTION ( 'NONE',  ( 0.000000000000000000, 0.000000000000000000, -1.000000000000000000 ) ) ;
#8917 = ADVANCED_FACE ( 'NONE', ( #5765 ), #15240, .T. ) ;
#8918 = CIRCLE ( 'NONE', #1300, 24.99999999999999645 ) ;
#8919 = CARTESIAN_POINT ( 'NONE',  ( 15.60228996708978855, 124.9392590763941371, 1.387778780781445676E-14 ) ) ;
#8920 = CARTESIAN_POINT ( 'NONE',  ( 34.79035048419334686, 200.2528945340144446, -20.13811431823772935 ) ) ;
#8921 = ORIENTED_EDGE ( 'NONE', *, *, #13073, .F. ) ;
#8922 = ADVANCED_FACE ( 'NONE', ( #4350 ), #4619, .T. ) ;
#8923 = CIRCLE ( 'NONE', #8081, 740.0000000000000000 ) ;
#8924 = EDGE_LOOP ( 'NONE', ( #5333, #17211, #17119, #10594 ) ) ;
#8925 = CARTESIAN_POINT ( 'NONE',  ( 19.14963388379468157, 19.99999999999999645, -24.55317681541820463 ) ) ;
#8926 = DIRECTION ( 'NONE',  ( 0.000000000000000000, 0.000000000000000000, -1.000000000000000000 ) ) ;
#8927 = ORIENTED_EDGE ( 'NONE', *, *, #4180, .T. ) ;
#8928 = DIRECTION ( 'NONE',  ( 0.000000000000000000, 2.775557561562891351E-15, -1.000000000000000000 ) ) ;
#8929 = CARTESIAN_POINT ( 'NONE',  ( 30.49999999999998224, 9.999999999999998224, 0.000000000000000000 ) ) ;
#8930 = AXIS2_PLACEMENT_3D ( 'NONE', #3660, #2239, #17291 ) ;
#8931 = VERTEX_POINT ( 'NONE', #7011 ) ;
#8932 = CARTESIAN_POINT ( 'NONE',  ( -208.0000000000000853, 170.0678595944000620, 2.693195258168412654 ) ) ;
#8933 = CARTESIAN_POINT ( 'NONE',  ( -77.50000000000001421, 196.6227766016838245, 0.000000000000000000 ) ) ;
#8934 = CARTESIAN_POINT ( 'NONE',  ( -45.00000000000000711, -20.00000000000000000, -35.00000000000000000 ) ) ;
#8935 = CARTESIAN_POINT ( 'NONE',  ( -10.72783954291835151, 17.99999999999999289, 10.92811494094397951 ) ) ;
#8936 = EDGE_CURVE ( 'NONE', #16407, #3419, #8216, .T. ) ;
#8937 = EDGE_CURVE ( 'NONE', #10732, #11377, #13716, .T. ) ;
#8938 = CARTESIAN_POINT ( 'NONE',  ( -27.99999999999998224, 10.00000000000000000, 10.00000000000000178 ) ) ;
#8939 = EDGE_CURVE ( 'NONE', #4720, #15136, #16998, .T. ) ;
#8940 = EDGE_CURVE ( 'NONE', #5255, #8340, #206, .T. ) ;
#8941 = AXIS2_PLACEMENT_3D ( 'NONE', #10812, #5757, #9732 ) ;
#8942 = DIRECTION ( 'NONE',  ( -1.000000000000000000, -6.938893903907228378E-16, -0.000000000000000000 ) ) ;
#8943 = AXIS2_PLACEMENT_3D ( 'NONE', #10819, #8070, #2682 ) ;
#8944 = ORIENTED_EDGE ( 'NONE', *, *, #11935, .F. ) ;
#8945 = FACE_OUTER_BOUND ( 'NONE', #15779, .T. ) ;
#8946 = VECTOR ( 'NONE', #10967, 1000.000000000000000 ) ;
#8947 = VERTEX_POINT ( 'NONE', #11075 ) ;
#8948 =( GEOMETRIC_REPRESENTATION_CONTEXT ( 3 ) GLOBAL_UNCERTAINTY_ASSIGNED_CONTEXT ( ( #12840 ) ) GLOBAL_UNIT_ASSIGNED_CONTEXT ( ( #15910, #14764, #15729 ) ) REPRESENTATION_CONTEXT ( 'NONE', 'WORKASPACE' ) );
#8949 = LINE ( 'NONE', #7790, #15818 ) ;
#8950 = VECTOR ( 'NONE', #1056, 1000.000000000000000 ) ;
#8951 = CARTESIAN_POINT ( 'NONE',  ( -70.00000000000000000, 171.6227766016838245, -20.00000000000000355 ) ) ;
#8952 = ORIENTED_EDGE ( 'NONE', *, *, #13345, .T. ) ;
#8953 = CARTESIAN_POINT ( 'NONE',  ( -27.98221281347037959, 30.00000000000000000, 0.000000000000000000 ) ) ;
#8954 = CARTESIAN_POINT ( 'NONE',  ( 16.61152767523464391, 142.9573811237880534, 16.36000751420521837 ) ) ;
#8955 = CARTESIAN_POINT ( 'NONE',  ( 24.52650527911658074, 19.99999999999999645, 8.254754350129561047 ) ) ;
#8956 = EDGE_LOOP ( 'NONE', ( #14944, #13979, #15431, #5439 ) ) ;
#8957 = AXIS2_PLACEMENT_3D ( 'NONE', #529, #13988, #5936 ) ;
#8958 = EDGE_CURVE ( 'NONE', #7262, #3754, #9358, .T. ) ;
#8959 = AXIS2_PLACEMENT_3D ( 'NONE', #3951, #11808, #17212 ) ;
#8960 = CYLINDRICAL_SURFACE ( 'NONE', #7519, 7.500000000000000000 ) ;
#8961 = PRESENTATION_LAYER_ASSIGNMENT (  '', '', ( #14076 ) ) ;
#8962 = CARTESIAN_POINT ( 'NONE',  ( 33.54345905997184474, 190.0067896460676309, -27.40528370530127233 ) ) ;
#8963 = DIRECTION ( 'NONE',  ( -0.000000000000000000, -0.000000000000000000, 1.000000000000000000 ) ) ;
#8964 = CARTESIAN_POINT ( 'NONE',  ( -10.22933296213221865, 30.92590585860461161, -12.59260918105267457 ) ) ;
#8965 = ORIENTED_EDGE ( 'NONE', *, *, #5271, .T. ) ;
#8966 = CARTESIAN_POINT ( 'NONE',  ( -43.00000000000000000, 138.6227766016838245, 0.000000000000000000 ) ) ;
#8967 = DIRECTION ( 'NONE',  ( 1.000000000000000000, -0.000000000000000000, -0.000000000000000000 ) ) ;
#8968 = ORIENTED_EDGE ( 'NONE', *, *, #11370, .T. ) ;
#8969 = CARTESIAN_POINT ( 'NONE',  ( 35.04511979140807654, 193.3541989604593141, -27.43934207688683813 ) ) ;
#8970 = DIRECTION ( 'NONE',  ( 0.000000000000000000, 0.000000000000000000, 1.000000000000000000 ) ) ;
#8971 = VERTEX_POINT ( 'NONE', #16490 ) ;
#8972 = AXIS2_PLACEMENT_3D ( 'NONE', #8212, #1311, #5298 ) ;
#8973 = EDGE_LOOP ( 'NONE', ( #5170, #7437, #15682, #5013 ) ) ;
#8974 = VERTEX_POINT ( 'NONE', #12765 ) ;
#8975 = PRODUCT_DEFINITION_FORMATION_WITH_SPECIFIED_SOURCE ( 'ANY', '', #5593, .NOT_KNOWN. ) ;
#8976 = AXIS2_PLACEMENT_3D ( 'NONE', #2478, #7963, #213 ) ;
#8977 = CARTESIAN_POINT ( 'NONE',  ( -77.72043220849697320, 153.7735974263995047, -27.75644086540375355 ) ) ;
#8978 = ORIENTED_EDGE ( 'NONE', *, *, #612, .T. ) ;
#8979 = EDGE_CURVE ( 'NONE', #4086, #5381, #2852, .T. ) ;
#8980 = CARTESIAN_POINT ( 'NONE',  ( 27.44407568426047561, 138.8271129316868837, -3.666666666666728247 ) ) ;
#8981 = EDGE_CURVE ( 'NONE', #13530, #4855, #16077, .T. ) ;
#8982 = DIRECTION ( 'NONE',  ( -1.000000000000000000, -0.000000000000000000, 0.000000000000000000 ) ) ;
#8983 = CARTESIAN_POINT ( 'NONE',  ( 30.89296198743065602, 152.5603119736738620, -29.35342143133167880 ) ) ;
#8984 = DIRECTION ( 'NONE',  ( -1.000000000000000000, 0.000000000000000000, 0.000000000000000000 ) ) ;
#8985 = VECTOR ( 'NONE', #1091, 999.9999999999998863 ) ;
#8986 = CIRCLE ( 'NONE', #17485, 2.500000000000002220 ) ;
#8987 = EDGE_LOOP ( 'NONE', ( #11064, #11121 ) ) ;
#8988 = DIRECTION ( 'NONE',  ( -0.08715574274764655016, -0.4980973490458782127, 0.8627299156628190913 ) ) ;
#8989 = LINE ( 'NONE', #15371, #8464 ) ;
#8990 = CARTESIAN_POINT ( 'NONE',  ( -206.3689767832464668, 166.7044760491588704, -0.5444864983988328966 ) ) ;
#8991 = CARTESIAN_POINT ( 'NONE',  ( 24.60077399342406679, 29.87270634359742871, 7.584611049657961068 ) ) ;
#8992 = ORIENTED_EDGE ( 'NONE', *, *, #10734, .T. ) ;
#8993 = CARTESIAN_POINT ( 'NONE',  ( -725.0000000000000000, 19.99999999999995737, 4.999999999999999112 ) ) ;
#8994 = EDGE_CURVE ( 'NONE', #9320, #7262, #11891, .T. ) ;
#8995 = CARTESIAN_POINT ( 'NONE',  ( -68.00000000000000000, 191.6227766016837961, 1.224646799147353454E-15 ) ) ;
#8996 = CIRCLE ( 'NONE', #238, 6.000000000000005329 ) ;
#8997 = ORIENTED_EDGE ( 'NONE', *, *, #12482, .F. ) ;
#8998 = CARTESIAN_POINT ( 'NONE',  ( -27.99999999999998224, 10.00000000000000000, -16.00000000000000000 ) ) ;
#9000 = CARTESIAN_POINT ( 'NONE',  ( 30.00000000000000355, 196.6227766016838245, -16.00000000000000000 ) ) ;
#8999 = VECTOR ( 'NONE', #16456, 1000.000000000000000 ) ;
#9001 = ORIENTED_EDGE ( 'NONE', *, *, #14791, .F. ) ;
#9002 = DIRECTION ( 'NONE',  ( 0.000000000000000000, 0.000000000000000000, 1.000000000000000000 ) ) ;
#9003 = CARTESIAN_POINT ( 'NONE',  ( 16.74904763372935790, 29.96341334642810139, -12.79227977592015897 ) ) ;
#9004 = CARTESIAN_POINT ( 'NONE',  ( -208.3486229709906752, 178.7173894086183168, 0.000000000000000000 ) ) ;
#9005 = CARTESIAN_POINT ( 'NONE',  ( -33.00000000000000711, 171.6227766016838245, 5.000000000000007994 ) ) ;
#9006 = ORIENTED_EDGE ( 'NONE', *, *, #5051, .F. ) ;
#9007 = DIRECTION ( 'NONE',  ( -1.000000000000000000, -0.000000000000000000, -0.000000000000000000 ) ) ;
#9008 = AXIS2_PLACEMENT_3D ( 'NONE', #2106, #7507, #13008 ) ;
#9009 = CARTESIAN_POINT ( 'NONE',  ( 1.559999999999998943, -0.8660254037844428154, -1.499999999999997780 ) ) ;
#9010 = AXIS2_PLACEMENT_3D ( 'NONE', #12795, #6060, #7214 ) ;
#9011 = LINE ( 'NONE', #11747, #787 ) ;
#9012 = CIRCLE ( 'NONE', #7330, 7.500000000000007105 ) ;
#9013 = CARTESIAN_POINT ( 'NONE',  ( 25.21468100261554568, 200.2598589880381610, -20.12830716182790169 ) ) ;
#9014 = EDGE_CURVE ( 'NONE', #14931, #15920, #4274, .T. ) ;
#9015 = ORIENTED_EDGE ( 'NONE', *, *, #5108, .F. ) ;
#9016 = ORIENTED_EDGE ( 'NONE', *, *, #15114, .F. ) ;
#9017 = CARTESIAN_POINT ( 'NONE',  ( 19.05951714192248403, 29.94485528828719367, -14.11495713418740294 ) ) ;
#9018 = CARTESIAN_POINT ( 'NONE',  ( 6.134011831684060390, 139.5514275721929209, -14.99999999999999822 ) ) ;
#9019 = VERTEX_POINT ( 'NONE', #222 ) ;
#9020 = CARTESIAN_POINT ( 'NONE',  ( -83.36213377134494351, 151.5968920417502090, -28.70510347301451404 ) ) ;
#9021 = CARTESIAN_POINT ( 'NONE',  ( 25.02538947966649729, 140.2588485512474392, -10.30263013689336304 ) ) ;
#9022 = VECTOR ( 'NONE', #14341, 1000.000000000000000 ) ;
#9023 = AXIS2_PLACEMENT_3D ( 'NONE', #10147, #7324, #4666 ) ;
#9024 = EDGE_LOOP ( 'NONE', ( #14639, #7957, #15699, #6494 ) ) ;
#9025 = ADVANCED_FACE ( 'NONE', ( #1546 ), #10761, .T. ) ;
#9026 = CIRCLE ( 'NONE', #7893, 2.500000000000002220 ) ;
#9027 = DIRECTION ( 'NONE',  ( 0.000000000000000000, 1.000000000000000000, 0.000000000000000000 ) ) ;
#9028 = CIRCLE ( 'NONE', #10440, 20.00000000000000355 ) ;
#9029 = DIRECTION ( 'NONE',  ( -1.000000000000000000, -0.000000000000000000, 0.000000000000000000 ) ) ;
#9030 = FACE_OUTER_BOUND ( 'NONE', #96, .T. ) ;
#9031 = DIRECTION ( 'NONE',  ( 0.000000000000000000, 0.000000000000000000, 1.000000000000000000 ) ) ;
#9032 = CARTESIAN_POINT ( 'NONE',  ( -25.16839285024616402, 18.00000000000000000, 15.12082343620105540 ) ) ;
#9033 = DIRECTION ( 'NONE',  ( -1.000000000000000000, -0.000000000000000000, 0.000000000000000000 ) ) ;
#9034 = DIRECTION ( 'NONE',  ( -1.000000000000000000, -0.000000000000000000, 0.000000000000000000 ) ) ;
#9035 = ORIENTED_EDGE ( 'NONE', *, *, #10734, .F. ) ;
#9036 = PLANE ( 'NONE',  #2214 ) ;
#9037 = CIRCLE ( 'NONE', #9608, 10.00000000000000000 ) ;
#9038 = VERTEX_POINT ( 'NONE', #13413 ) ;
#9039 = CARTESIAN_POINT ( 'NONE',  ( -197.9999999999999716, 171.6227766016838245, 0.000000000000000000 ) ) ;
#9040 = AXIS2_PLACEMENT_3D ( 'NONE', #9380, #3724, #9027 ) ;
#9041 = DIRECTION ( 'NONE',  ( 0.000000000000000000, -1.000000000000000000, 0.000000000000000000 ) ) ;
#9042 = VERTEX_POINT ( 'NONE', #8185 ) ;
#9043 = CARTESIAN_POINT ( 'NONE',  ( 34.93420767853316988, 20.00000000000000000, 4.999999999999999112 ) ) ;
#9044 = CARTESIAN_POINT ( 'NONE',  ( 7.290380404777190293, 133.8591131982526008, 12.94327073059132971 ) ) ;
#9045 = EDGE_CURVE ( 'NONE', #570, #16427, #8792, .T. ) ;
#9046 = EDGE_CURVE ( 'NONE', #17091, #3368, #6866, .T. ) ;
#9047 = CARTESIAN_POINT ( 'NONE',  ( 34.26467700469002864, 19.99999999999999645, 10.17319632352553427 ) ) ;
#9048 = EDGE_CURVE ( 'NONE', #17253, #16339, #10667, .T. ) ;
#9049 = CIRCLE ( 'NONE', #10453, 33.00000000000000000 ) ;
#9050 = VECTOR ( 'NONE', #15372, 1000.000000000000000 ) ;
#9051 = ORIENTED_EDGE ( 'NONE', *, *, #4252, .F. ) ;
#9052 = CARTESIAN_POINT ( 'NONE',  ( -32.66708739526796279, 101.0743273401215419, 4.648823768412004398 ) ) ;
#9053 = CARTESIAN_POINT ( 'NONE',  ( 2.950000000000001066, 0.000000000000000000, 0.000000000000000000 ) ) ;
#9054 = CARTESIAN_POINT ( 'NONE',  ( -17.19488518268993715, 32.09742631896689602, -9.330173263366075886 ) ) ;
#9055 = CARTESIAN_POINT ( 'NONE',  ( -27.98221281347032274, 18.00000000000000000, -4.999999999999996447 ) ) ;
#9056 = ORIENTED_EDGE ( 'NONE', *, *, #364, .F. ) ;
#9057 = CARTESIAN_POINT ( 'NONE',  ( -24.99999999999999645, 120.0000000000000284, -4.999999999999999112 ) ) ;
#9058 = EDGE_LOOP ( 'NONE', ( #5077, #6905, #10220, #11040 ) ) ;
#9059 = DIRECTION ( 'NONE',  ( -1.000000000000000000, 0.000000000000000000, 0.000000000000000000 ) ) ;
#9060 = DIRECTION ( 'NONE',  ( 1.000000000000000000, 0.000000000000000000, -0.000000000000000000 ) ) ;
#9061 = AXIS2_PLACEMENT_3D ( 'NONE', #2882, #227, #7046 ) ;
#9062 = ORIENTED_EDGE ( 'NONE', *, *, #12167, .F. ) ;
#9063 = VERTEX_POINT ( 'NONE', #14655 ) ;
#9064 = ORIENTED_EDGE ( 'NONE', *, *, #607, .F. ) ;
#9065 = CARTESIAN_POINT ( 'NONE',  ( -73.01962815379008020, 149.3990418665993332, -24.40116746791568758 ) ) ;
#9066 = EDGE_LOOP ( 'NONE', ( #756, #15028, #7686, #8247 ) ) ;
#9067 = CARTESIAN_POINT ( 'NONE',  ( 0.000000000000000000, 0.000000000000000000, 0.000000000000000000 ) ) ;
#9068 = CARTESIAN_POINT ( 'NONE',  ( -14.96200682865387854, 32.37632742624003157, 9.274234733431431010 ) ) ;
#9069 = CARTESIAN_POINT ( 'NONE',  ( -27.99999999999998224, 10.00000000000000000, 0.000000000000000000 ) ) ;
#9070 = VECTOR ( 'NONE', #3141, 1000.000000000000000 ) ;
#9071 = LINE ( 'NONE', #16733, #11774 ) ;
#9072 = CARTESIAN_POINT ( 'NONE',  ( 13.66341101665266677, 138.6227766016838245, 1.000341871676679184E-14 ) ) ;
#9073 = ORIENTED_EDGE ( 'NONE', *, *, #935, .F. ) ;
#9074 = DIRECTION ( 'NONE',  ( 0.000000000000000000, 1.000000000000000000, 0.000000000000000000 ) ) ;
#9075 = CARTESIAN_POINT ( 'NONE',  ( 17.53512989260226362, 29.96507997281579350, -14.66107963853301399 ) ) ;
#9076 = DIRECTION ( 'NONE',  ( -1.000000000000000000, 0.000000000000000000, 0.000000000000000000 ) ) ;
#9077 = CARTESIAN_POINT ( 'NONE',  ( 30.81698523721487604, 18.00000000000000000, 17.17210857557096659 ) ) ;
#9078 = CARTESIAN_POINT ( 'NONE',  ( 39.99999999999998579, 20.00000000000000000, -30.00000000000001066 ) ) ;
#9079 = ORIENTED_EDGE ( 'NONE', *, *, #14638, .T. ) ;
#9080 = DIRECTION ( 'NONE',  ( -1.000000000000000000, 0.000000000000000000, 0.000000000000000000 ) ) ;
#9081 = EDGE_CURVE ( 'NONE', #8664, #14798, #3427, .T. ) ;
#9082 = AXIS2_PLACEMENT_3D ( 'NONE', #17374, #10647, #15243 ) ;
#9083 = CARTESIAN_POINT ( 'NONE',  ( 34.99999999999999289, 197.2379877313571797, 20.82664773619436360 ) ) ;
#9084 = ORIENTED_EDGE ( 'NONE', *, *, #11698, .T. ) ;
#9085 = CARTESIAN_POINT ( 'NONE',  ( -32.55406425504676093, 100.5254706298718901, -5.163900856522908533 ) ) ;
#9086 = DIRECTION ( 'NONE',  ( 0.000000000000000000, 0.000000000000000000, -1.000000000000000000 ) ) ;
#9087 = ORIENTED_EDGE ( 'NONE', *, *, #8736, .T. ) ;
#9088 =( NAMED_UNIT ( * ) PLANE_ANGLE_UNIT ( ) SI_UNIT ( $, .RADIAN. ) );
#9089 = DIRECTION ( 'NONE',  ( 0.000000000000000000, 0.000000000000000000, 1.000000000000000000 ) ) ;
#9090 = DIRECTION ( 'NONE',  ( 0.000000000000000000, 0.000000000000000000, 1.000000000000000000 ) ) ;
#9091 = CARTESIAN_POINT ( 'NONE',  ( -74.65470611475511475, 143.8751093726684473, -21.33821933965574758 ) ) ;
#9092 = DIRECTION ( 'NONE',  ( 1.000000000000000000, 0.000000000000000000, 0.000000000000000000 ) ) ;
#9093 = VERTEX_POINT ( 'NONE', #14749 ) ;
#9094 = DIRECTION ( 'NONE',  ( 0.000000000000000000, 0.000000000000000000, -1.000000000000000000 ) ) ;
#9095 = CARTESIAN_POINT ( 'NONE',  ( 6.134011831684049731, 144.1839557653416080, 18.33333333333335702 ) ) ;
#9096 = DIRECTION ( 'NONE',  ( 0.000000000000000000, 0.000000000000000000, -1.000000000000000000 ) ) ;
#9097 = CARTESIAN_POINT ( 'NONE',  ( 24.50594157886344959, 199.0592542586747697, -21.73717956246133909 ) ) ;
#9098 = ORIENTED_EDGE ( 'NONE', *, *, #11645, .F. ) ;
#9099 = EDGE_LOOP ( 'NONE', ( #9887, #7476 ) ) ;
#9100 = ADVANCED_FACE ( 'NONE', ( #2876 ), #2620, .T. ) ;
#9101 = VERTEX_POINT ( 'NONE', #1285 ) ;
#9102 = ADVANCED_BREP_SHAPE_REPRESENTATION ( '', ( #5407, #3583 ), #17150 ) ;
#9103 = CARTESIAN_POINT ( 'NONE',  ( 18.30724418481576166, 140.7653321920888345, -16.52022657272140904 ) ) ;
#9104 = ORIENTED_EDGE ( 'NONE', *, *, #9353, .T. ) ;
#9105 = DIRECTION ( 'NONE',  ( -1.000000000000000000, 0.000000000000000000, 0.000000000000000000 ) ) ;
#9106 = CARTESIAN_POINT ( 'NONE',  ( 8.431728255697246155, 133.2562109147605156, -12.71722808757355949 ) ) ;
#9107 = EDGE_CURVE ( 'NONE', #5512, #8410, #15588, .T. ) ;
#9108 = ORIENTED_EDGE ( 'NONE', *, *, #16711, .T. ) ;
#9109 = CARTESIAN_POINT ( 'NONE',  ( 30.00000000000000355, 196.6227766016838245, -16.00000000000000000 ) ) ;
#9110 = LINE ( 'NONE', #8046, #13864 ) ;
#9111 = EDGE_CURVE ( 'NONE', #1757, #7915, #6787, .T. ) ;
#9112 = EDGE_CURVE ( 'NONE', #15090, #2144, #12086, .T. ) ;
#9113 = DIRECTION ( 'NONE',  ( 0.9961946980917465444, -0.04357787137382451714, 0.07547908730516460218 ) ) ;
#9114 = DIRECTION ( 'NONE',  ( -1.000000000000000000, -0.000000000000000000, -0.000000000000000000 ) ) ;
#9115 = DIRECTION ( 'NONE',  ( -1.000000000000000000, 0.000000000000000000, 0.000000000000000000 ) ) ;
#9116 = CARTESIAN_POINT ( 'NONE',  ( -8.509631953695096840, 18.00000000000455103, 12.55445085332768151 ) ) ;
#9117 = CYLINDRICAL_SURFACE ( 'NONE', #7751, 2.500000000000000444 ) ;
#9118 = FACE_OUTER_BOUND ( 'NONE', #6507, .T. ) ;
#9119 = ORIENTED_EDGE ( 'NONE', *, *, #15904, .T. ) ;
#9120 = FACE_OUTER_BOUND ( 'NONE', #6013, .T. ) ;
#9121 = ORIENTED_EDGE ( 'NONE', *, *, #7691, .F. ) ;
#9122 = DIRECTION ( 'NONE',  ( -0.000000000000000000, -1.000000000000000000, -0.000000000000000000 ) ) ;
#9123 = CARTESIAN_POINT ( 'NONE',  ( -13.90980987654338286, 18.00000000000000355, -23.98326992096529864 ) ) ;
#9124 = APPLICATION_CONTEXT ( 'automotive_design' ) ;
#9125 = ORIENTED_EDGE ( 'NONE', *, *, #14371, .T. ) ;
#9126 = DIRECTION ( 'NONE',  ( -1.000000000000000000, 0.000000000000000000, 0.000000000000000000 ) ) ;
#9127 = CARTESIAN_POINT ( 'NONE',  ( 15.26338903195270547, 125.9505563168691111, 6.751637631526196337 ) ) ;
#9128 = EDGE_LOOP ( 'NONE', ( #3668, #12856 ) ) ;
#9129 = CARTESIAN_POINT ( 'NONE',  ( -100.0000000000000000, 171.6227766016838245, 27.69059892324149530 ) ) ;
#9130 = VERTEX_POINT ( 'NONE', #131 ) ;
#9131 = DIRECTION ( 'NONE',  ( 0.000000000000000000, 0.8660254037844380415, 0.5000000000000011102 ) ) ;
#9132 = CARTESIAN_POINT ( 'NONE',  ( 27.72043220849692702, 189.4719557769681444, -27.75644086540374644 ) ) ;
#9133 = DIRECTION ( 'NONE',  ( 0.000000000000000000, 0.000000000000000000, 1.000000000000000000 ) ) ;
#9134 = CARTESIAN_POINT ( 'NONE',  ( -14.45029498972267668, 32.22448475281832003, -9.930813566224275135 ) ) ;
#9135 = ORIENTED_EDGE ( 'NONE', *, *, #9747, .T. ) ;
#9136 = FACE_OUTER_BOUND ( 'NONE', #9765, .T. ) ;
#9137 = EDGE_CURVE ( 'NONE', #8198, #5744, #5129, .T. ) ;
#9138 = EDGE_CURVE ( 'NONE', #16166, #7981, #6828, .T. ) ;
#9139 = ADVANCED_FACE ( 'NONE', ( #13332, #5367, #16344 ), #12182, .F. ) ;
#9140 = ORIENTED_EDGE ( 'NONE', *, *, #14669, .T. ) ;
#9141 = CARTESIAN_POINT ( 'NONE',  ( 34.31461291909280220, 192.4344680579923761, -28.14280641908791480 ) ) ;
#9142 = CARTESIAN_POINT ( 'NONE',  ( -85.59781103574918859, 201.6348411963793410, -13.74530841833676220 ) ) ;
#9143 = ORIENTED_EDGE ( 'NONE', *, *, #9927, .T. ) ;
#9144 = ORIENTED_EDGE ( 'NONE', *, *, #11523, .T. ) ;
#9145 = ORIENTED_EDGE ( 'NONE', *, *, #3705, .F. ) ;
#9146 = CARTESIAN_POINT ( 'NONE',  ( -82.79368516360898411, 153.6052450214444605, -27.64877209012308867 ) ) ;
#9147 = UNCERTAINTY_MEASURE_WITH_UNIT (LENGTH_MEASURE( 1.000000000000000082E-05 ), #2199, 'distance_accuracy_value', 'NONE');
#9148 = ORIENTED_EDGE ( 'NONE', *, *, #2990, .F. ) ;
#9149 = DIRECTION ( 'NONE',  ( 0.000000000000000000, 0.000000000000000000, 1.000000000000000000 ) ) ;
#9150 = FACE_BOUND ( 'NONE', #163, .T. ) ;
#9151 = CARTESIAN_POINT ( 'NONE',  ( -8.730345434444062747, 30.30576128541687453, 14.94291915632153334 ) ) ;
#9152 =( BOUNDED_SURFACE ( )  B_SPLINE_SURFACE ( 3, 2, ( 
 ( #3740, #2401, #14625 ),
 ( #17365, #10637, #16045 ),
 ( #13118, #13209, #3922 ),
 ( #2595, #14453, #7982 ),
 ( #13383, #12054, #5424 ),
 ( #17462, #5334, #1251 ),
 ( #6659, #10729, #16143 ),
 ( #4017, #14799, #8061 ),
 ( #13475, #1350, #6753 ),
 ( #12150, #21, #10814 ),
 ( #6386, #2319, #17189 ),
 ( #5064, #10460, #6909 ),
 ( #8317, #3107, #5848 ),
 ( #2926, #5503, #276 ),
 ( #9651, #4178, #15133 ),
 ( #4442, #2847, #12230 ),
 ( #187, #1697, #4269 ),
 ( #1779, #439, #13832 ),
 ( #13917, #2764, #15049 ),
 ( #16662, #12309, #14970 ),
 ( #7007, #11244, #16404 ),
 ( #1515, #5590, #9827 ),
 ( #10981, #9471, #8154 ),
 ( #359, #13731, #13568 ) ),
 .UNSPECIFIED., .F., .F., .F. ) 
 B_SPLINE_SURFACE_WITH_KNOTS ( ( 4, 2, 2, 2, 2, 2, 2, 2, 2, 2, 2, 4 ),
 ( 3, 3 ),
 ( 0.01427588378380419132, 0.01824401167166925936, 0.02022807561560179684, 0.02221213955953433086, 0.02618026744739940237, 0.02816433139133193639, 0.03014839533526447041, 0.03411652322312953844, 0.03610058716706207593, 0.03808465111099461342, 0.04205277899885968146, 0.04602090688672474950 ),
 ( 0.000000000000000000, 1.000000000000000000 ),
 .UNSPECIFIED. ) 
 GEOMETRIC_REPRESENTATION_ITEM ( )  RATIONAL_B_SPLINE_SURFACE ( (
 ( 1.000000000000000000, 0.7071067811865476838, 1.000000000000000000),
 ( 1.000000000000000000, 0.7013659285814082267, 1.000000000000000000),
 ( 1.000000000000000000, 0.6957352470443716186, 1.000000000000000000),
 ( 1.000000000000000000, 0.6874449304735253952, 1.000000000000000000),
 ( 1.000000000000000000, 0.6847075230359779274, 1.000000000000000000),
 ( 1.000000000000000000, 0.6792848743381553200, 1.000000000000000000),
 ( 1.000000000000000000, 0.6765866164121365767, 1.000000000000000000),
 ( 1.000000000000000000, 0.6687223666254397125, 1.000000000000000000),
 ( 1.000000000000000000, 0.6637534122518267132, 1.000000000000000000),
 ( 1.000000000000000000, 0.6567012635110727192, 1.000000000000000000),
 ( 1.000000000000000000, 0.6544178910915308123, 1.000000000000000000),
 ( 1.000000000000000000, 0.6499901663949341213, 1.000000000000000000),
 ( 1.000000000000000000, 0.6478648508491323676, 1.000000000000000000),
 ( 1.000000000000000000, 0.6418284244073564349, 1.000000000000000000),
 ( 1.000000000000000000, 0.6382188548936990058, 1.000000000000000000),
 ( 1.000000000000000000, 0.6334349500989927551, 1.000000000000000000),
 ( 1.000000000000000000, 0.6319385063094495880, 1.000000000000000000),
 ( 1.000000000000000000, 0.6292162870119188955, 1.000000000000000000),
 ( 1.000000000000000000, 0.6279881568154176419, 1.000000000000000000),
 ( 1.000000000000000000, 0.6246939197237179053, 1.000000000000000000),
 ( 1.000000000000000000, 0.6230139244305938906, 1.000000000000000000),
 ( 1.000000000000000000, 0.6207349535630983794, 1.000000000000000000),
 ( 1.000000000000000000, 0.6201739322037901347, 1.000000000000000000),
 ( 1.000000000000000000, 0.6201736729460421982, 1.000000000000000000) ) ) 
 REPRESENTATION_ITEM ( '' )  SURFACE ( )  );
#9153 = CARTESIAN_POINT ( 'NONE',  ( 39.99999999999999289, 20.00000000000000000, 0.000000000000000000 ) ) ;
#9154 = CARTESIAN_POINT ( 'NONE',  ( 21.54590827305403877, 18.00000000000000000, 9.735228713654757726 ) ) ;
#9155 = FACE_OUTER_BOUND ( 'NONE', #1510, .T. ) ;
#9156 = AXIS2_PLACEMENT_3D ( 'NONE', #348, #8668, #1767 ) ;
#9157 = EDGE_LOOP ( 'NONE', ( #11222, #8156, #3536, #4578, #1363 ) ) ;
#9158 = PLANE ( 'NONE',  #16895 ) ;
#9159 = LINE ( 'NONE', #9662, #4932 ) ;
#9160 = EDGE_CURVE ( 'NONE', #8796, #11521, #17007, .T. ) ;
#9161 = EDGE_CURVE ( 'NONE', #8531, #8768, #1734, .T. ) ;
#9163 = FACE_OUTER_BOUND ( 'NONE', #6211, .T. ) ;
#9162 = VECTOR ( 'NONE', #8703, 1000.000000000000000 ) ;
#9164 = CARTESIAN_POINT ( 'NONE',  ( 34.26588824652853305, 18.00000000000000000, 10.16858984204336736 ) ) ;
#9165 = CARTESIAN_POINT ( 'NONE',  ( -27.84784281930893357, 19.99999999999999645, -7.647248539284095870 ) ) ;
#9166 = EDGE_CURVE ( 'NONE', #4908, #13584, #14122, .T. ) ;
#9167 = VERTEX_POINT ( 'NONE', #9770 ) ;
#9168 = DIRECTION ( 'NONE',  ( -0.000000000000000000, 0.000000000000000000, -1.000000000000000000 ) ) ;
#9169 = CARTESIAN_POINT ( 'NONE',  ( 29.05191969268358321, 201.5373699728807537, 13.93281245758937992 ) ) ;
#9170 = VERTEX_POINT ( 'NONE', #8354 ) ;
#9171 = SURFACE_SIDE_STYLE ('',( #5288 ) ) ;
#9172 = CARTESIAN_POINT ( 'NONE',  ( -27.99999999999998224, 10.00000000000000000, 0.000000000000000000 ) ) ;
#9173 = AXIS2_PLACEMENT_3D ( 'NONE', #3813, #11679, #10353 ) ;
#9174 = ORIENTED_EDGE ( 'NONE', *, *, #17265, .T. ) ;
#9175 = CARTESIAN_POINT ( 'NONE',  ( -82.68880486155467224, 142.3932571782017646, 15.32207027268389865 ) ) ;
#9176 = VECTOR ( 'NONE', #10883, 1000.000000000000000 ) ;
#9177 = DIRECTION ( 'NONE',  ( -0.8571673013836867971, 0.000000000000000000, -0.5150380737757237481 ) ) ;
#9178 = FACE_OUTER_BOUND ( 'NONE', #16507, .T. ) ;
#9179 = EDGE_CURVE ( 'NONE', #10705, #7796, #9368, .T. ) ;
#9180 = CARTESIAN_POINT ( 'NONE',  ( -206.3689767832464668, 166.7044760491588704, -0.5444864983988328966 ) ) ;
#9181 = ORIENTED_EDGE ( 'NONE', *, *, #11547, .F. ) ;
#9182 = DIRECTION ( 'NONE',  ( 1.000000000000000000, 0.000000000000000000, 0.000000000000000000 ) ) ;
#9183 = CARTESIAN_POINT ( 'NONE',  ( -207.7508999721942757, 173.1946085995199667, -5.195646985528586725 ) ) ;
#9184 = FACE_OUTER_BOUND ( 'NONE', #12526, .T. ) ;
#9185 = CARTESIAN_POINT ( 'NONE',  ( -82.50000000000002842, 146.6227766016838245, 1.387778780781445676E-14 ) ) ;
#9186 = AXIS2_PLACEMENT_3D ( 'NONE', #5196, #14582, #1040 ) ;
#9187 = CIRCLE ( 'NONE', #4955, 5.000000000000004441 ) ;
#9188 = VERTEX_POINT ( 'NONE', #311 ) ;
#9189 = ORIENTED_EDGE ( 'NONE', *, *, #14906, .F. ) ;
#9190 = CIRCLE ( 'NONE', #7228, 2.000000000000001776 ) ;
#9191 = LINE ( 'NONE', #13361, #12924 ) ;
#9192 = ORIENTED_EDGE ( 'NONE', *, *, #17062, .F. ) ;
#9193 = CARTESIAN_POINT ( 'NONE',  ( -85.14000932857697990, 149.7234947166294603, -27.30319596934542048 ) ) ;
#9194 = CARTESIAN_POINT ( 'NONE',  ( 21.38051303318334462, 141.6185065902053282, -13.74313897096208414 ) ) ;
#9195 = ORIENTED_EDGE ( 'NONE', *, *, #11943, .T. ) ;
#9196 = CARTESIAN_POINT ( 'NONE',  ( -187.6513770290095238, 172.4976050944027008, 4.898587196589412829E-16 ) ) ;
#9197 = FACE_OUTER_BOUND ( 'NONE', #12851, .T. ) ;
#9198 = VECTOR ( 'NONE', #2171, 1000.000000000000000 ) ;
#9199 = CARTESIAN_POINT ( 'NONE',  ( -192.9999999999999716, 171.6227766016838245, 0.000000000000000000 ) ) ;
#9200 = CARTESIAN_POINT ( 'NONE',  ( -102.0000000000000142, 171.6227766016838245, -28.26633746182137585 ) ) ;
#9201 = EDGE_CURVE ( 'NONE', #6832, #5595, #9859, .T. ) ;
#9202 = VECTOR ( 'NONE', #16430, 1000.000000000000000 ) ;
#9203 = DIRECTION ( 'NONE',  ( 1.000000000000000000, 0.000000000000000000, 0.000000000000000000 ) ) ;
#9204 = CARTESIAN_POINT ( 'NONE',  ( 22.88332935572807969, 29.84310215611307271, -6.048604702147989620 ) ) ;
#9205 = FACE_OUTER_BOUND ( 'NONE', #3950, .T. ) ;
#9206 = CARTESIAN_POINT ( 'NONE',  ( -23.00000000000000000, 120.0000000000000284, -15.00000000000000000 ) ) ;
#9207 = DIRECTION ( 'NONE',  ( 1.000000000000000000, 0.000000000000000000, -0.000000000000000000 ) ) ;
#9208 = ORIENTED_EDGE ( 'NONE', *, *, #572, .T. ) ;
#9209 = CARTESIAN_POINT ( 'NONE',  ( 16.97539380423070909, 126.5649914159620266, -7.928130581088665529 ) ) ;
#9210 = ORIENTED_EDGE ( 'NONE', *, *, #6385, .F. ) ;
#9211 = EDGE_CURVE ( 'NONE', #8681, #1349, #11618, .T. ) ;
#9212 = DIRECTION ( 'NONE',  ( 1.000000000000000000, 0.000000000000000000, 0.000000000000000000 ) ) ;
#9213 = EDGE_CURVE ( 'NONE', #3385, #5700, #15080, .T. ) ;
#9214 = DIRECTION ( 'NONE',  ( -1.000000000000000000, 0.000000000000000000, 0.000000000000000000 ) ) ;
#9215 = VECTOR ( 'NONE', #10477, 1000.000000000000000 ) ;
#9216 = ORIENTED_EDGE ( 'NONE', *, *, #144, .F. ) ;
#9217 = CARTESIAN_POINT ( 'NONE',  ( -80.00000000000002842, 146.6227766016838245, -16.00000000000000000 ) ) ;
#9218 = CARTESIAN_POINT ( 'NONE',  ( 14.12141184870282196, 138.6801925718470443, 3.743222489502259887 ) ) ;
#9219 = ORIENTED_EDGE ( 'NONE', *, *, #14530, .F. ) ;
#9220 = CARTESIAN_POINT ( 'NONE',  ( 17.04731744882672828, 19.99999999999885247, 14.80421929169553685 ) ) ;
#9221 = VERTEX_POINT ( 'NONE', #4561 ) ;
#9222 = CARTESIAN_POINT ( 'NONE',  ( -27.99999999999998224, 10.00000000000000000, -35.00200000000000244 ) ) ;
#9223 = AXIS2_PLACEMENT_3D ( 'NONE', #4867, #12571, #11412 ) ;
#9224 = VECTOR ( 'NONE', #4188, 1000.000000000000000 ) ;
#9225 = CARTESIAN_POINT ( 'NONE',  ( 27.99239453806529099, 189.3908747183072592, -27.80828541846619828 ) ) ;
#9226 = FACE_OUTER_BOUND ( 'NONE', #1700, .T. ) ;
#9227 = AXIS2_PLACEMENT_3D ( 'NONE', #12133, #7966, #1153 ) ;
#9228 = CARTESIAN_POINT ( 'NONE',  ( -20.86241502029199424, 18.00000000000000000, -20.14618526197082460 ) ) ;
#9229 = AXIS2_PLACEMENT_3D ( 'NONE', #14091, #631, #7606 ) ;
#9230 = EDGE_LOOP ( 'NONE', ( #10524, #15538, #11141, #2600 ) ) ;
#9231 = CARTESIAN_POINT ( 'NONE',  ( 33.96623626252291928, 149.6716700844112324, 24.64096846353361414 ) ) ;
#9232 = EDGE_LOOP ( 'NONE', ( #808, #12771, #6877 ) ) ;
#9233 = CARTESIAN_POINT ( 'NONE',  ( 26.63661590110499233, 191.6363561590497966, -28.71510896997970264 ) ) ;
#9234 = LINE ( 'NONE', #14546, #5263 ) ;
#9235 = ADVANCED_FACE ( 'NONE', ( #9947 ), #656, .T. ) ;
#9236 = VERTEX_POINT ( 'NONE', #11099 ) ;
#9237 = ORIENTED_EDGE ( 'NONE', *, *, #12954, .T. ) ;
#9238 = VERTEX_POINT ( 'NONE', #1989 ) ;
#9240 = CARTESIAN_POINT ( 'NONE',  ( -78.54584381417873828, 153.9859494455611468, -27.89172594985639364 ) ) ;
#9239 = STYLED_ITEM ( 'NONE', ( #327 ), #16081 ) ;
#9241 =( GEOMETRIC_REPRESENTATION_CONTEXT ( 3 ) GLOBAL_UNCERTAINTY_ASSIGNED_CONTEXT ( ( #17426 ) ) GLOBAL_UNIT_ASSIGNED_CONTEXT ( ( #3157, #16874, #9789 ) ) REPRESENTATION_CONTEXT ( 'NONE', 'WORKASPACE' ) );
#9242 = ORIENTED_EDGE ( 'NONE', *, *, #1103, .F. ) ;
#9243 = CARTESIAN_POINT ( 'NONE',  ( 0.000000000000000000, 0.000000000000000000, 0.000000000000000000 ) ) ;
#9244 = EDGE_CURVE ( 'NONE', #16546, #11799, #9638, .T. ) ;
#9245 = CARTESIAN_POINT ( 'NONE',  ( -10.05738114656989346, 30.87167111307020306, 12.65386873594253103 ) ) ;
#9246 = CARTESIAN_POINT ( 'NONE',  ( -17.86279820300995169, 32.23061541110773476, 7.751589558536285729 ) ) ;
#9247 = CARTESIAN_POINT ( 'NONE',  ( 24.02490146132329940, 147.2612100285404608, -25.13395616064557103 ) ) ;
#9248 = DIRECTION ( 'NONE',  ( 1.000000000000000000, 0.000000000000000000, 0.000000000000000000 ) ) ;
#9249 = CARTESIAN_POINT ( 'NONE',  ( -82.57145418340599008, 150.9146311475675759, 25.69413650784049707 ) ) ;
#9250 = VERTEX_POINT ( 'NONE', #7293 ) ;
#9251 = CARTESIAN_POINT ( 'NONE',  ( -168.0000000000000284, 168.3180863238817437, 5.723891464432140808 ) ) ;
#9252 = CARTESIAN_POINT ( 'NONE',  ( -31.66708739526795924, 120.0000000000000284, 5.500000000000000000 ) ) ;
#9253 = AXIS2_PLACEMENT_3D ( 'NONE', #939, #2537, #9074 ) ;
#9254 = FACE_OUTER_BOUND ( 'NONE', #6265, .T. ) ;
#9255 = PRODUCT_DEFINITION_FORMATION_WITH_SPECIFIED_SOURCE ( 'ANY', '', #4183, .NOT_KNOWN. ) ;
#9256 = CARTESIAN_POINT ( 'NONE',  ( 25.51458778375578973, 18.00000000000000000, 21.98440010584615578 ) ) ;
#9257 = FACE_OUTER_BOUND ( 'NONE', #2315, .T. ) ;
#9258 = ORIENTED_EDGE ( 'NONE', *, *, #8884, .F. ) ;
#9259 = CARTESIAN_POINT ( 'NONE',  ( 34.93420767853316988, 20.00000000000000000, -15.00000000000000000 ) ) ;
#9260 = CARTESIAN_POINT ( 'NONE',  ( 32.67866620718707082, 200.8588467739806447, 15.30956876290918522 ) ) ;
#9261 = ORIENTED_EDGE ( 'NONE', *, *, #13345, .F. ) ;
#9262 = LINE ( 'NONE', #2550, #16964 ) ;
#9263 = EDGE_LOOP ( 'NONE', ( #13654, #493, #3652, #17284 ) ) ;
#9264 = EDGE_CURVE ( 'NONE', #12122, #2736, #2019, .T. ) ;
#9265 = EDGE_CURVE ( 'NONE', #8108, #4701, #5976, .T. ) ;
#9266 = CIRCLE ( 'NONE', #9834, 2.500000000000002220 ) ;
#9267 = CYLINDRICAL_SURFACE ( 'NONE', #2558, 4.000000000000003553 ) ;
#9268 = EDGE_CURVE ( 'NONE', #11936, #15042, #13867, .T. ) ;
#9269 = AXIS2_PLACEMENT_3D ( 'NONE', #9545, #2999, #12387 ) ;
#9270 = CARTESIAN_POINT ( 'NONE',  ( 34.99999999999999289, -20.00000000000000000, 34.99999999999999289 ) ) ;
#9271 = LINE ( 'NONE', #5292, #2503 ) ;
#9272 = CARTESIAN_POINT ( 'NONE',  ( -10.03891356649071653, 19.99999999999999289, 24.87483525495232328 ) ) ;
#9273 = ORIENTED_EDGE ( 'NONE', *, *, #10741, .T. ) ;
#9274 = DIRECTION ( 'NONE',  ( 0.000000000000000000, 0.000000000000000000, -1.000000000000000000 ) ) ;
#9275 = CARTESIAN_POINT ( 'NONE',  ( -207.6775903968322439, 173.2516151616937350, -5.122575873392639423 ) ) ;
#9276 = DIRECTION ( 'NONE',  ( -1.000000000000000000, 0.000000000000000000, 0.000000000000000000 ) ) ;
#9277 = CARTESIAN_POINT ( 'NONE',  ( 35.99999999999999289, 196.9987679943316721, -24.11115281963766321 ) ) ;
#9278 = CIRCLE ( 'NONE', #3925, 2.500000000000002220 ) ;
#9279 = CIRCLE ( 'NONE', #15516, 5.000000000000004441 ) ;
#9280 = ORIENTED_EDGE ( 'NONE', *, *, #9973, .T. ) ;
#9281 = CARTESIAN_POINT ( 'NONE',  ( 8.904477399772744661, 142.4465447428235620, -19.33413753149157088 ) ) ;
#9282 = EDGE_LOOP ( 'NONE', ( #4440, #9663, #11600, #5369 ) ) ;
#9283 = DIRECTION ( 'NONE',  ( -1.000000000000000000, -0.000000000000000000, 0.000000000000000000 ) ) ;
#9284 = CARTESIAN_POINT ( 'NONE',  ( 14.44088586081352688, 138.6571688462224472, -6.678806037552732278 ) ) ;
#9285 = VERTEX_POINT ( 'NONE', #16512 ) ;
#9286 = LINE ( 'NONE', #7872, #11240 ) ;
#9287 = CARTESIAN_POINT ( 'NONE',  ( 0.000000000000000000, 0.8660254037844428154, -1.499999999999997780 ) ) ;
#9288 = DIRECTION ( 'NONE',  ( 0.000000000000000000, 0.000000000000000000, -1.000000000000000000 ) ) ;
#9289 = CIRCLE ( 'NONE', #16664, 2.500000000000000000 ) ;
#9290 = EDGE_CURVE ( 'NONE', #10702, #11548, #8637, .T. ) ;
#9291 = VECTOR ( 'NONE', #4051, 1000.000000000000000 ) ;
#9292 = DIRECTION ( 'NONE',  ( 0.000000000000000000, 0.000000000000000000, -1.000000000000000000 ) ) ;
#9293 = CIRCLE ( 'NONE', #12703, 35.00000000000000000 ) ;
#9294 = CARTESIAN_POINT ( 'NONE',  ( -45.00000000000003553, 120.0000000000000142, 4.999999999999999112 ) ) ;
#9295 = CARTESIAN_POINT ( 'NONE',  ( 34.26467700469002153, 18.00000000000000000, -10.17319632352554137 ) ) ;
#9296 = CARTESIAN_POINT ( 'NONE',  ( -7.379000772445021283, 30.00000000000000000, -25.00000000000000000 ) ) ;
#9297 = DIRECTION ( 'NONE',  ( -1.000000000000000000, -0.000000000000000000, -0.000000000000000000 ) ) ;
#9298 = DIRECTION ( 'NONE',  ( -0.000000000000000000, -0.000000000000000000, -1.000000000000000000 ) ) ;
#9299 = DIRECTION ( 'NONE',  ( -0.000000000000000000, -0.000000000000000000, -1.000000000000000000 ) ) ;
#9300 = ORIENTED_EDGE ( 'NONE', *, *, #7565, .F. ) ;
#9301 = CARTESIAN_POINT ( 'NONE',  ( 6.134011831684053284, 134.2062027339443944, 25.00000000000000000 ) ) ;
#9302 = EDGE_LOOP ( 'NONE', ( #13324, #11398, #1049, #12552, #14493 ) ) ;
#9303 = DIRECTION ( 'NONE',  ( -0.000000000000000000, -0.000000000000000000, -1.000000000000000000 ) ) ;
#9304 = DIRECTION ( 'NONE',  ( 1.000000000000000000, 0.000000000000000000, 0.000000000000000000 ) ) ;
#9305 = AXIS2_PLACEMENT_3D ( 'NONE', #6379, #4883, #11778 ) ;
#9306 = ORIENTED_EDGE ( 'NONE', *, *, #4888, .F. ) ;
#9307 = EDGE_CURVE ( 'NONE', #16699, #9960, #15347, .T. ) ;
#9308 = DIRECTION ( 'NONE',  ( -0.000000000000000000, -0.000000000000000000, -1.000000000000000000 ) ) ;
#9309 = VECTOR ( 'NONE', #4374, 1000.000000000000000 ) ;
#9310 = CARTESIAN_POINT ( 'NONE',  ( 13.90347339350139677, 138.7488974902626069, 3.510692536284492959 ) ) ;
#9311 = VERTEX_POINT ( 'NONE', #6053 ) ;
#9312 = LINE ( 'NONE', #1083, #11015 ) ;
#9313 = VERTEX_POINT ( 'NONE', #15174 ) ;
#9314 = CARTESIAN_POINT ( 'NONE',  ( -30.49999999999998224, 10.00000000000000000, -16.00000000000000000 ) ) ;
#9315 = CARTESIAN_POINT ( 'NONE',  ( 22.74907522843311369, 194.6587679740005115, -23.63587233142071042 ) ) ;
#9316 = AXIS2_PLACEMENT_3D ( 'NONE', #11842, #15743, #14503 ) ;
#9317 = LINE ( 'NONE', #3933, #12764 ) ;
#9318 = CARTESIAN_POINT ( 'NONE',  ( -19.80886414215282798, 18.00000000000000000, -20.97268729564153489 ) ) ;
#9319 = AXIS2_PLACEMENT_3D ( 'NONE', #10798, #967, #17346 ) ;
#9320 = VERTEX_POINT ( 'NONE', #3045 ) ;
#9321 = CARTESIAN_POINT ( 'NONE',  ( 34.53513972622751993, 148.7497411309094275, 23.78985390322973359 ) ) ;
#9322 = VERTEX_POINT ( 'NONE', #7202 ) ;
#9323 = CARTESIAN_POINT ( 'NONE',  ( -76.45654094002816237, 190.0067896460675740, -27.40528370530127233 ) ) ;
#9324 = DIRECTION ( 'NONE',  ( -0.000000000000000000, 1.000000000000000000, 8.673617379884035472E-16 ) ) ;
#9325 = ORIENTED_EDGE ( 'NONE', *, *, #3253, .F. ) ;
#9326 = VERTEX_POINT ( 'NONE', #16777 ) ;
#9327 = ORIENTED_EDGE ( 'NONE', *, *, #8606, .T. ) ;
#9328 = EDGE_CURVE ( 'NONE', #5404, #6861, #15436, .T. ) ;
#9329 = VECTOR ( 'NONE', #1657, 1000.000000000000000 ) ;
#9330 = AXIS2_PLACEMENT_3D ( 'NONE', #684, #2090, #2351 ) ;
#9331 = CARTESIAN_POINT ( 'NONE',  ( -80.00000000000001421, 196.6227766016838245, 35.00200000000000244 ) ) ;
#9332 = CIRCLE ( 'NONE', #14165, 6.000000000000005329 ) ;
#9333 = ADVANCED_FACE ( 'NONE', ( #5787 ), #17283, .T. ) ;
#9334 = VERTEX_POINT ( 'NONE', #8713 ) ;
#9335 = DIRECTION ( 'NONE',  ( -1.000000000000000000, 0.000000000000000000, 0.000000000000000000 ) ) ;
#9336 = DIRECTION ( 'NONE',  ( -0.000000000000000000, -0.000000000000000000, -1.000000000000000000 ) ) ;
#9337 = EDGE_CURVE ( 'NONE', #6998, #3217, #3715, .T. ) ;
#9338 =( LENGTH_UNIT ( ) NAMED_UNIT ( * ) SI_UNIT ( .MILLI., .METRE. ) );
#9339 = EDGE_CURVE ( 'NONE', #10807, #1310, #14278, .T. ) ;
#9340 = CARTESIAN_POINT ( 'NONE',  ( 24.44272481504117778, 148.9119151679986430, -26.63478011418836644 ) ) ;
#9341 = CARTESIAN_POINT ( 'NONE',  ( 49.99999999999998579, 159.6227766016838814, 5.571800142134975431 ) ) ;
#9342 = CYLINDRICAL_SURFACE ( 'NONE', #15409, 33.00000000000000000 ) ;
#9343 = ORIENTED_EDGE ( 'NONE', *, *, #15326, .T. ) ;
#9344 = DIRECTION ( 'NONE',  ( -1.000000000000000000, -0.000000000000000000, -0.000000000000000000 ) ) ;
#9345 = AXIS2_PLACEMENT_3D ( 'NONE', #7363, #11153, #12498 ) ;
#9346 = CARTESIAN_POINT ( 'NONE',  ( 19.36310082087489803, 29.94084738964976111, -13.97143931599698874 ) ) ;
#9347 = CARTESIAN_POINT ( 'NONE',  ( 12.53348921593948972, 131.0729685438566605, 13.11561688552428784 ) ) ;
#9348 = DIRECTION ( 'NONE',  ( -1.000000000000000000, 0.000000000000000000, 2.312964634635742464E-16 ) ) ;
#9349 = AXIS2_PLACEMENT_3D ( 'NONE', #8002, #12083, #1281 ) ;
#9350 = LINE ( 'NONE', #16180, #3364 ) ;
#9351 = ORIENTED_EDGE ( 'NONE', *, *, #15095, .F. ) ;
#9352 = CARTESIAN_POINT ( 'NONE',  ( 48.00000000000000711, 151.6227766016839098, 8.071800142134973655 ) ) ;
#9353 = EDGE_CURVE ( 'NONE', #14104, #6709, #11581, .T. ) ;
#9354 = DIRECTION ( 'NONE',  ( -1.156482317317868274E-16, 1.000000000000000000, -0.000000000000000000 ) ) ;
#9355 = CYLINDRICAL_SURFACE ( 'NONE', #13876, 20.00000000000000355 ) ;
#9356 = ORIENTED_EDGE ( 'NONE', *, *, #3253, .T. ) ;
#9357 = SURFACE_STYLE_USAGE ( .BOTH. , #16095 ) ;
#9358 = CIRCLE ( 'NONE', #10478, 149.9999999999999716 ) ;
#9359 = EDGE_LOOP ( 'NONE', ( #8639, #37, #1732, #14874 ) ) ;
#9360 = CARTESIAN_POINT ( 'NONE',  ( -75.00000000000002842, 146.6227766016838245, 21.54065922853802562 ) ) ;
#9361 = CARTESIAN_POINT ( 'NONE',  ( 16.23725950538872809, 18.00000000000000000, -24.99999999982344789 ) ) ;
#9362 = CARTESIAN_POINT ( 'NONE',  ( -84.32132260856947426, 142.4452037501735902, -19.33642647557002192 ) ) ;
#9363 = CARTESIAN_POINT ( 'NONE',  ( 30.00000000000001066, 146.6227766016838245, -35.00200000000000244 ) ) ;
#9364 = ORIENTED_EDGE ( 'NONE', *, *, #11493, .F. ) ;
#9365 = FACE_OUTER_BOUND ( 'NONE', #12442, .T. ) ;
#9366 = DIRECTION ( 'NONE',  ( -1.000000000000000000, 0.000000000000000000, 0.000000000000000000 ) ) ;
#9367 = FACE_OUTER_BOUND ( 'NONE', #10179, .T. ) ;
#9368 = CIRCLE ( 'NONE', #2597, 2.500000000000000444 ) ;
#9369 = PRODUCT_DEFINITION_CONTEXT ( 'detailed design', #2580, 'design' ) ;
#9370 = EDGE_CURVE ( 'NONE', #11161, #16720, #7394, .T. ) ;
#9371 = EDGE_CURVE ( 'NONE', #8437, #10436, #11536, .T. ) ;
#9372 = EDGE_CURVE ( 'NONE', #12169, #817, #887, .T. ) ;
#9373 = ORIENTED_EDGE ( 'NONE', *, *, #5274, .T. ) ;
#9374 = CARTESIAN_POINT ( 'NONE',  ( 16.26529498815335373, 136.8354558863973409, -4.782531348471686705 ) ) ;
#9375 = ORIENTED_EDGE ( 'NONE', *, *, #14637, .T. ) ;
#9376 = CARTESIAN_POINT ( 'NONE',  ( -85.77867439187610898, 148.2463666031633238, -26.04982723689806434 ) ) ;
#9377 = CARTESIAN_POINT ( 'NONE',  ( 25.87766738269754541, 139.8661988410599406, -8.984976992518891592 ) ) ;
#9378 = EDGE_LOOP ( 'NONE', ( #10295, #15333, #17499, #12104 ) ) ;
#9379 = CARTESIAN_POINT ( 'NONE',  ( -206.3689767832464668, 174.5534660175772785, 3.987129972734268168 ) ) ;
#9380 = CARTESIAN_POINT ( 'NONE',  ( 48.00000000000000711, 187.6227766016837961, 12.50000337241049309 ) ) ;
#9381 = DIRECTION ( 'NONE',  ( -1.000000000000000000, -0.000000000000000000, 0.000000000000000000 ) ) ;
#9382 = DIRECTION ( 'NONE',  ( 1.000000000000000000, 0.000000000000000000, 0.000000000000000000 ) ) ;
#9383 = CARTESIAN_POINT ( 'NONE',  ( -95.00000000000000000, 201.6227766016838245, 1.836970198721029589E-15 ) ) ;
#9384 = CARTESIAN_POINT ( 'NONE',  ( 28.14717441101696593, 18.00000000000000000, -20.07001214884044415 ) ) ;
#9385 = DIRECTION ( 'NONE',  ( 1.000000000000000000, 0.000000000000000000, 0.000000000000000000 ) ) ;
#9386 = FACE_OUTER_BOUND ( 'NONE', #11761, .T. ) ;
#9387 = LINE ( 'NONE', #8144, #13860 ) ;
#9388 = CARTESIAN_POINT ( 'NONE',  ( -95.00000000000000000, 171.6227766016838245, 0.000000000000000000 ) ) ;
#9389 = ORIENTED_EDGE ( 'NONE', *, *, #2107, .F. ) ;
#9390 = CARTESIAN_POINT ( 'NONE',  ( -208.0000000000000853, 170.0678595944000620, 2.693195258168412654 ) ) ;
#9391 = EDGE_CURVE ( 'NONE', #2665, #6230, #14185, .T. ) ;
#9392 = VERTEX_POINT ( 'NONE', #17108 ) ;
#9393 = DIRECTION ( 'NONE',  ( -2.312964634635742464E-16, 0.000000000000000000, 1.000000000000000000 ) ) ;
#9394 = FACE_OUTER_BOUND ( 'NONE', #8520, .T. ) ;
#9395 = EDGE_LOOP ( 'NONE', ( #1933, #8110 ) ) ;
#9396 = CYLINDRICAL_SURFACE ( 'NONE', #10002, 2.500000000000002220 ) ;
#9397 = CARTESIAN_POINT ( 'NONE',  ( 21.84350049701177809, 141.4638053371992328, 13.40107808329819150 ) ) ;
#9398 = ORIENTED_EDGE ( 'NONE', *, *, #3100, .F. ) ;
#9399 = CARTESIAN_POINT ( 'NONE',  ( 18.45742352454476887, 29.95282391178955095, 14.36414658362611974 ) ) ;
#9400 = ORIENTED_EDGE ( 'NONE', *, *, #6199, .T. ) ;
#9401 = FACE_OUTER_BOUND ( 'NONE', #2518, .T. ) ;
#9402 = CARTESIAN_POINT ( 'NONE',  ( -95.00000000000000000, 171.6227766016838245, -27.69059892324149530 ) ) ;
#9403 = DIRECTION ( 'NONE',  ( -1.000000000000000000, -0.000000000000000000, 0.000000000000000000 ) ) ;
#9404 = CARTESIAN_POINT ( 'NONE',  ( -3.000000000000000888, 154.3022685259950038, -9.999999999999900524 ) ) ;
#9405 = ADVANCED_FACE ( 'NONE', ( #6304, #3746 ), #7636, .F. ) ;
#9406 = ORIENTED_EDGE ( 'NONE', *, *, #3975, .T. ) ;
#9407 = CARTESIAN_POINT ( 'NONE',  ( 26.33723719015080889, 150.0417915422717101, 24.96744664354709897 ) ) ;
#9408 = ORIENTED_EDGE ( 'NONE', *, *, #3162, .T. ) ;
#9409 = CARTESIAN_POINT ( 'NONE',  ( -87.25092477156692894, 194.6587679740005115, -23.63587233142071042 ) ) ;
#9410 = CARTESIAN_POINT ( 'NONE',  ( -87.20996884815647832, 198.7539484232961513, -18.80562413441371206 ) ) ;
#9411 = EDGE_LOOP ( 'NONE', ( #14619, #11595, #7105, #4631 ) ) ;
#9412 = ORIENTED_EDGE ( 'NONE', *, *, #17363, .T. ) ;
#9413 = ORIENTED_EDGE ( 'NONE', *, *, #3078, .F. ) ;
#9414 = DIRECTION ( 'NONE',  ( -1.000000000000000000, 0.000000000000000000, 0.000000000000000000 ) ) ;
#9415 = ORIENTED_EDGE ( 'NONE', *, *, #10825, .F. ) ;
#9416 = ITEM_DEFINED_TRANSFORMATION ( 'NONE', 'NONE', #775,  #3583 ) ;
#9417 = CARTESIAN_POINT ( 'NONE',  ( 48.00000000000000711, 159.6227766016838814, 5.571800142134975431 ) ) ;
#9418 = DIRECTION ( 'NONE',  ( 1.000000000000000000, 0.000000000000000000, 0.000000000000000000 ) ) ;
#9419 = CARTESIAN_POINT ( 'NONE',  ( -31.89848094669885725, 100.0271397714182342, 5.500000000000000000 ) ) ;
#9420 = DIRECTION ( 'NONE',  ( 1.000000000000000000, 0.000000000000000000, 0.000000000000000000 ) ) ;
#9421 = CARTESIAN_POINT ( 'NONE',  ( -75.10310273927775881, 147.6679082027615948, 22.70058015389365735 ) ) ;
#9422 = EDGE_CURVE ( 'NONE', #8896, #14332, #16453, .T. ) ;
#9423 = ORIENTED_EDGE ( 'NONE', *, *, #9244, .F. ) ;
#9424 = CARTESIAN_POINT ( 'NONE',  ( -84.06062570790729183, 201.0559264674919291, -18.94433901724533342 ) ) ;
#9425 = DIRECTION ( 'NONE',  ( -1.000000000000000000, -0.000000000000000000, -0.000000000000000000 ) ) ;
#9426 = CARTESIAN_POINT ( 'NONE',  ( 20.13757169487763576, 18.00000000000000000, 24.32197800972832624 ) ) ;
#9427 = CARTESIAN_POINT ( 'NONE',  ( -207.7491074081026170, 173.1961128903347173, 5.193772935353458742 ) ) ;
#9428 = DIRECTION ( 'NONE',  ( -1.000000000000000000, 0.000000000000000000, 0.000000000000000000 ) ) ;
#9429 = ADVANCED_FACE ( 'NONE', ( #7457 ), #745, .T. ) ;
#9430 = EDGE_CURVE ( 'NONE', #2922, #1718, #7109, .T. ) ;
#9431 = DIRECTION ( 'NONE',  ( 0.000000000000000000, 0.000000000000000000, 1.000000000000000000 ) ) ;
#9432 = ORIENTED_EDGE ( 'NONE', *, *, #13820, .F. ) ;
#9433 = DIRECTION ( 'NONE',  ( -1.000000000000000000, -0.000000000000000000, 0.000000000000000000 ) ) ;
#9434 = VERTEX_POINT ( 'NONE', #12866 ) ;
#9435 = FACE_OUTER_BOUND ( 'NONE', #14140, .T. ) ;
#9436 = CARTESIAN_POINT ( 'NONE',  ( 48.00000000000000711, 146.6227766016838245, 4.592425496802573578E-15 ) ) ;
#9437 = CARTESIAN_POINT ( 'NONE',  ( -86.00000000000002842, 146.6227766016838245, -24.49489742783179480 ) ) ;
#9438 = DIRECTION ( 'NONE',  ( 0.000000000000000000, 0.000000000000000000, 1.000000000000000000 ) ) ;
#9439 = ORIENTED_EDGE ( 'NONE', *, *, #1193, .F. ) ;
#9440 = DIRECTION ( 'NONE',  ( 0.000000000000000000, 0.000000000000000000, -1.000000000000000000 ) ) ;
#9441 = DIRECTION ( 'NONE',  ( 1.000000000000000000, 0.000000000000000000, -0.000000000000000000 ) ) ;
#9442 = CARTESIAN_POINT ( 'NONE',  ( -34.99999999999999289, 122.0000000000000284, -4.999999999999999112 ) ) ;
#9443 = CARTESIAN_POINT ( 'NONE',  ( 35.96514256823365940, 197.3601060891146517, -23.72478281133074773 ) ) ;
#9444 = PRODUCT_RELATED_PRODUCT_CATEGORY ( 'part', '', ( #4765 ) ) ;
#9445 = CIRCLE ( 'NONE', #17381, 5.000000000000000888 ) ;
#9446 = CARTESIAN_POINT ( 'NONE',  ( 16.64812168497169864, 126.9869021000460663, -8.626120676703536105 ) ) ;
#9447 = AXIS2_PLACEMENT_3D ( 'NONE', #3384, #9034, #14264 ) ;
#9448 = ORIENTED_EDGE ( 'NONE', *, *, #10562, .T. ) ;
#9449 = DIRECTION ( 'NONE',  ( 0.000000000000000000, 0.000000000000000000, 1.000000000000000000 ) ) ;
#9450 = DIRECTION ( 'NONE',  ( -0.000000000000000000, -0.000000000000000000, 1.000000000000000000 ) ) ;
#9451 = EDGE_LOOP ( 'NONE', ( #7283, #4316, #17367, #13968, #3166, #17280, #2525, #7006, #15250, #6957, #6154, #5754, #6405, #8298, #5175 ) ) ;
#9452 = FACE_OUTER_BOUND ( 'NONE', #4230, .T. ) ;
#9453 = CARTESIAN_POINT ( 'NONE',  ( -85.41098039551273757, 194.0039740083362858, -26.91197613625889673 ) ) ;
#9454 = CARTESIAN_POINT ( 'NONE',  ( 17.00000000000000000, 191.6227766016837961, 1.224646799147353454E-15 ) ) ;
#9455 = EDGE_CURVE ( 'NONE', #16020, #2717, #6142, .T. ) ;
#9456 = CARTESIAN_POINT ( 'NONE',  ( 30.00000000000001066, 146.6227766016838245, -12.99999999999999822 ) ) ;
#9457 = CARTESIAN_POINT ( 'NONE',  ( 29.98123639043839006, 18.00000000000000000, -18.19121573219640098 ) ) ;
#9458 = CIRCLE ( 'NONE', #4398, 750.0000000000001137 ) ;
#9459 = CARTESIAN_POINT ( 'NONE',  ( 19.20424459521615290, 18.00000000000228439, -11.86908137778077688 ) ) ;
#9460 = CARTESIAN_POINT ( 'NONE',  ( 34.93420767853318409, 30.00000000000000000, -5.000000000000010658 ) ) ;
#9461 = CARTESIAN_POINT ( 'NONE',  ( -5.000000000000004441, 171.6227766016838245, 0.000000000000000000 ) ) ;
#9462 =( GEOMETRIC_REPRESENTATION_CONTEXT ( 3 ) GLOBAL_UNCERTAINTY_ASSIGNED_CONTEXT ( ( #10564 ) ) GLOBAL_UNIT_ASSIGNED_CONTEXT ( ( #7255, #12487, #3187 ) ) REPRESENTATION_CONTEXT ( 'NONE', 'WORKASPACE' ) );
#9463 = DIRECTION ( 'NONE',  ( -1.000000000000000000, -0.000000000000000000, -0.000000000000000000 ) ) ;
#9464 = CARTESIAN_POINT ( 'NONE',  ( 24.26049027360500432, 144.8396561671642360, -22.53731575973597501 ) ) ;
#9465 = VERTEX_POINT ( 'NONE', #16152 ) ;
#9466 = DIRECTION ( 'NONE',  ( -1.000000000000000000, -0.000000000000000000, 0.000000000000000000 ) ) ;
#9467 = VERTEX_POINT ( 'NONE', #10549 ) ;
#9468 = FACE_OUTER_BOUND ( 'NONE', #17344, .T. ) ;
#9469 = CARTESIAN_POINT ( 'NONE',  ( -116.4755503550297107, 171.6227766016838245, 0.000000000000000000 ) ) ;
#9470 = ORIENTED_EDGE ( 'NONE', *, *, #9430, .F. ) ;
#9471 = CARTESIAN_POINT ( 'NONE',  ( -15.33310217281858634, 19.99999999999769784, 5.462585411291380311 ) ) ;
#9472 = CARTESIAN_POINT ( 'NONE',  ( 25.02538947966649729, 140.2588485512474392, 10.30263013689336304 ) ) ;
#9473 = AXIS2_PLACEMENT_3D ( 'NONE', #7142, #13794, #12541 ) ;
#9474 = VERTEX_POINT ( 'NONE', #13484 ) ;
#9475 = CIRCLE ( 'NONE', #10331, 248.0000000000000000 ) ;
#9476 = CARTESIAN_POINT ( 'NONE',  ( 17.20984524040877872, 19.99999999999999645, 14.76996962246643896 ) ) ;
#9477 = AXIS2_PLACEMENT_3D ( 'NONE', #7144, #14058, #13890 ) ;
#9478 = ORIENTED_EDGE ( 'NONE', *, *, #3927, .F. ) ;
#9479 = EDGE_CURVE ( 'NONE', #5469, #17135, #9317, .T. ) ;
#9480 = EDGE_CURVE ( 'NONE', #10541, #7474, #14344, .T. ) ;
#9481 = EDGE_CURVE ( 'NONE', #14947, #9019, #15957, .T. ) ;
#9482 = EDGE_CURVE ( 'NONE', #6730, #7936, #8807, .T. ) ;
#9483 = DIRECTION ( 'NONE',  ( -1.000000000000000000, -0.000000000000000000, -0.000000000000000000 ) ) ;
#9484 = CARTESIAN_POINT ( 'NONE',  ( 34.46470488465457294, 190.5906835324045119, -27.00480063125523600 ) ) ;
#9485 = DIRECTION ( 'NONE',  ( 0.000000000000000000, 1.000000000000000000, 0.000000000000000000 ) ) ;
#9486 = DIRECTION ( 'NONE',  ( -0.000000000000000000, -0.000000000000000000, -1.000000000000000000 ) ) ;
#9487 = AXIS2_PLACEMENT_3D ( 'NONE', #14823, #13507, #10838 ) ;
#9488 = ORIENTED_EDGE ( 'NONE', *, *, #10638, .T. ) ;
#9489 = DIRECTION ( 'NONE',  ( -1.000000000000000000, 0.000000000000000000, 0.000000000000000000 ) ) ;
#9490 = CIRCLE ( 'NONE', #747, 12.00000000000000000 ) ;
#9491 = ORIENTED_EDGE ( 'NONE', *, *, #14606, .T. ) ;
#9492 = CARTESIAN_POINT ( 'NONE',  ( 48.00000000000000711, 191.6227766016837677, -5.571800142134975431 ) ) ;
#9493 = LINE ( 'NONE', #1529, #9787 ) ;
#9494 = CARTESIAN_POINT ( 'NONE',  ( -100.0000000000000000, 171.6227766016838245, 0.000000000000000000 ) ) ;
#9495 = ORIENTED_EDGE ( 'NONE', *, *, #6514, .F. ) ;
#9496 = EDGE_LOOP ( 'NONE', ( #6240, #14112, #10036 ) ) ;
#9497 = CARTESIAN_POINT ( 'NONE',  ( 7.535032041485008492, 142.5209969262061804, 19.44444444359253410 ) ) ;
#9498 = AXIS2_PLACEMENT_3D ( 'NONE', #9469, #4176, #4091 ) ;
#9499 = CIRCLE ( 'NONE', #452, 2.499999999999998668 ) ;
#9500 = ORIENTED_EDGE ( 'NONE', *, *, #6341, .T. ) ;
#9501 = APPLICATION_PROTOCOL_DEFINITION ( 'draft international standard', 'automotive_design', 1998, #3142 ) ;
#9502 = FACE_OUTER_BOUND ( 'NONE', #11357, .T. ) ;
#9503 = VECTOR ( 'NONE', #9780, 1000.000000000000000 ) ;
#9504 = DIRECTION ( 'NONE',  ( -0.000000000000000000, -0.000000000000000000, -1.000000000000000000 ) ) ;
#9505 = CARTESIAN_POINT ( 'NONE',  ( 21.87945022329474298, 29.86245334106958538, -9.005757899690800983 ) ) ;
#9506 = DIRECTION ( 'NONE',  ( 0.000000000000000000, 0.000000000000000000, -1.000000000000000000 ) ) ;
#9507 = CARTESIAN_POINT ( 'NONE',  ( -75.00000000000004263, 146.8780590376976249, 21.83693896782702026 ) ) ;
#9508 = ORIENTED_EDGE ( 'NONE', *, *, #11007, .F. ) ;
#9509 = CARTESIAN_POINT ( 'NONE',  ( -50.00000000000000000, 171.6227766016838245, -2.602085213965210642E-15 ) ) ;
#9510 = CARTESIAN_POINT ( 'NONE',  ( -87.50000000000004263, 196.6227766016838245, -13.00000000000000000 ) ) ;
#9511 = CARTESIAN_POINT ( 'NONE',  ( 14.93242934743711992, 20.00000000000000000, -25.00000000000000000 ) ) ;
#9512 = CARTESIAN_POINT ( 'NONE',  ( -207.9324504923922632, 173.0008837612440402, 5.418295114331532325 ) ) ;
#9513 = DIRECTION ( 'NONE',  ( -1.000000000000000000, 0.000000000000000000, 0.000000000000000000 ) ) ;
#9514 = CIRCLE ( 'NONE', #1891, 747.9999999999998863 ) ;
#9515 = ORIENTED_EDGE ( 'NONE', *, *, #15169, .F. ) ;
#9516 = AXIS2_PLACEMENT_3D ( 'NONE', #14611, #1066, #4821 ) ;
#9517 = AXIS2_PLACEMENT_3D ( 'NONE', #1190, #854, #2258 ) ;
#9518 = AXIS2_PLACEMENT_3D ( 'NONE', #1497, #16283, #10867 ) ;
#9519 = LINE ( 'NONE', #1480, #1980 ) ;
#9520 = EDGE_CURVE ( 'NONE', #874, #1820, #5413, .T. ) ;
#9521 = EDGE_LOOP ( 'NONE', ( #2981, #10816, #5152, #7322 ) ) ;
#9522 = ADVANCED_FACE ( 'NONE', ( #6763 ), #7989, .T. ) ;
#9523 = CARTESIAN_POINT ( 'NONE',  ( -22.93725393319379435, 100.0000000000000142, -6.000000000000000000 ) ) ;
#9524 = ORIENTED_EDGE ( 'NONE', *, *, #11054, .F. ) ;
#9525 = CARTESIAN_POINT ( 'NONE',  ( 17.56954167074719919, 125.3114906870353167, -3.338394383324010395 ) ) ;
#9526 = DIRECTION ( 'NONE',  ( 0.000000000000000000, 0.000000000000000000, 1.000000000000000000 ) ) ;
#9527 = CARTESIAN_POINT ( 'NONE',  ( 4.755015822784812052, 0.000000000000000000, 0.000000000000000000 ) ) ;
#9528 = AXIS2_PLACEMENT_3D ( 'NONE', #3184, #11328, #618 ) ;
#9529 = EDGE_CURVE ( 'NONE', #16965, #3735, #14729, .T. ) ;
#9530 = AXIS2_PLACEMENT_3D ( 'NONE', #5726, #7221, #6068 ) ;
#9531 = ORIENTED_EDGE ( 'NONE', *, *, #15171, .T. ) ;
#9532 = EDGE_CURVE ( 'NONE', #3735, #15620, #11060, .T. ) ;
#9533 = DIRECTION ( 'NONE',  ( -1.000000000000000000, 0.000000000000000000, 0.000000000000000000 ) ) ;
#9534 = DIRECTION ( 'NONE',  ( 1.000000000000000000, 0.000000000000000000, 0.000000000000000000 ) ) ;
#9535 = CARTESIAN_POINT ( 'NONE',  ( -68.00000000000000000, 171.6227766016838245, -2.296212748401287183E-15 ) ) ;
#9536 = CARTESIAN_POINT ( 'NONE',  ( -147.9615242270661213, 171.6227766016838245, 0.000000000000000000 ) ) ;
#9537 = CARTESIAN_POINT ( 'NONE',  ( -40.00000000000000000, 20.00000000000000000, -30.00000000000000355 ) ) ;
#9538 = AXIS2_PLACEMENT_3D ( 'NONE', #8291, #13699, #12546 ) ;
#9539 = ORIENTED_EDGE ( 'NONE', *, *, #34, .F. ) ;
#9540 = FACE_BOUND ( 'NONE', #7020, .T. ) ;
#9541 = CARTESIAN_POINT ( 'NONE',  ( 27.42233521511133887, 138.9393305618597481, -4.670371664028303726 ) ) ;
#9542 = ORIENTED_EDGE ( 'NONE', *, *, #15204, .T. ) ;
#9543 = FILL_AREA_STYLE ('',( #343 ) ) ;
#9544 = DIRECTION ( 'NONE',  ( 0.000000000000000000, 0.000000000000000000, -1.000000000000000000 ) ) ;
#9545 = CARTESIAN_POINT ( 'NONE',  ( -100.0000000000000000, 171.6227766016838245, 0.000000000000000000 ) ) ;
#9546 = CARTESIAN_POINT ( 'NONE',  ( 25.93409701014191882, 193.6946896392258282, 24.53450862945287980 ) ) ;
#9547 = EDGE_CURVE ( 'NONE', #13466, #11970, #10739, .T. ) ;
#9548 = CARTESIAN_POINT ( 'NONE',  ( 34.93420767853316988, 18.00000000000000355, -4.999999999999999112 ) ) ;
#9549 = ADVANCED_FACE ( 'NONE', ( #3836 ), #13579, .F. ) ;
#9550 = CARTESIAN_POINT ( 'NONE',  ( 17.52334770333193248, 18.00000000000227018, -12.62810114740270606 ) ) ;
#9551 = CARTESIAN_POINT ( 'NONE',  ( -31.66708739526795924, 119.0000000000000284, -5.500000000000000000 ) ) ;
#9552 = CARTESIAN_POINT ( 'NONE',  ( 17.51497691750854813, 29.94811823131043127, 12.57651788136221072 ) ) ;
#9553 = AXIS2_PLACEMENT_3D ( 'NONE', #15786, #10376, #14640 ) ;
#9554 = LINE ( 'NONE', #14960, #3401 ) ;
#9555 = CIRCLE ( 'NONE', #13810, 2.499999999999998668 ) ;
#9556 = FILL_AREA_STYLE_COLOUR ( '', #10293 ) ;
#9557 = EDGE_LOOP ( 'NONE', ( #1580, #14889 ) ) ;
#9558 = CARTESIAN_POINT ( 'NONE',  ( 17.54349574104648823, 125.4948194589026684, -4.999999999999997335 ) ) ;
#9559 = EDGE_LOOP ( 'NONE', ( #5609, #13165, #7256, #2030, #2694 ) ) ;
#9560 = CARTESIAN_POINT ( 'NONE',  ( 49.99999999999998579, 159.6227766016838814, 5.571800142134975431 ) ) ;
#9561 = DIRECTION ( 'NONE',  ( 1.000000000000000000, 0.000000000000000000, 0.000000000000000000 ) ) ;
#9562 = EDGE_CURVE ( 'NONE', #11405, #6602, #12159, .T. ) ;
#9563 = ORIENTED_EDGE ( 'NONE', *, *, #14841, .T. ) ;
#9564 = DIRECTION ( 'NONE',  ( 0.000000000000000000, -0.4999999999999952816, -0.8660254037844413721 ) ) ;
#9565 = CARTESIAN_POINT ( 'NONE',  ( -725.0000000000000000, 30.00000000000000000, -25.00000000000000000 ) ) ;
#9566 = ORIENTED_EDGE ( 'NONE', *, *, #6492, .F. ) ;
#9567 = VECTOR ( 'NONE', #17184, 1000.000000000000000 ) ;
#9568 = CARTESIAN_POINT ( 'NONE',  ( 26.45654094002815526, 153.2387635573001319, -27.40528370530127233 ) ) ;
#9569 = AXIS2_PLACEMENT_3D ( 'NONE', #9964, #5997, #11560 ) ;
#9570 = ORIENTED_EDGE ( 'NONE', *, *, #5123, .T. ) ;
#9571 = LINE ( 'NONE', #14976, #7532 ) ;
#9572 = CARTESIAN_POINT ( 'NONE',  ( -725.0000000000000000, 19.99999999999995737, -13.00000000000000000 ) ) ;
#9573 = CARTESIAN_POINT ( 'NONE',  ( 0.000000000000000000, 0.000000000000000000, 4.750000000000000000 ) ) ;
#9574 = EDGE_LOOP ( 'NONE', ( #3693, #16958, #2608, #15967, #2301, #15440 ) ) ;
#9575 = DIRECTION ( 'NONE',  ( 0.000000000000000000, 0.000000000000000000, 1.000000000000000000 ) ) ;
#9576 = EDGE_LOOP ( 'NONE', ( #8245, #6179, #9706, #5895 ) ) ;
#9577 = CARTESIAN_POINT ( 'NONE',  ( 32.06470260736958267, 151.1803749979462737, 25.90597399044990823 ) ) ;
#9578 = CIRCLE ( 'NONE', #7891, 12.00000000000000000 ) ;
#9579 = VERTEX_POINT ( 'NONE', #1522 ) ;
#9580 = DIRECTION ( 'NONE',  ( -0.000000000000000000, -0.000000000000000000, -1.000000000000000000 ) ) ;
#9581 = AXIS2_PLACEMENT_3D ( 'NONE', #6785, #1729, #5712 ) ;
#9582 = DIRECTION ( 'NONE',  ( 0.000000000000000000, 0.000000000000000000, -1.000000000000000000 ) ) ;
#9583 = B_SPLINE_CURVE_WITH_KNOTS ( 'NONE', 3,
 ( #4452, #14102, #10191, #15244, #15331, #4627, #3291, #1964, #450, #14189 ),
 .UNSPECIFIED., .F., .F.,
 ( 4, 2, 2, 2, 4 ),
 ( 0.0003067249959486639528, 0.0007024845516937828528, 0.001098244107438901915, 0.001494003663184020761, 0.001889763218929139824 ),
 .UNSPECIFIED. ) ;
#9584 = EDGE_CURVE ( 'NONE', #7981, #16166, #13051, .T. ) ;
#9585 = CARTESIAN_POINT ( 'NONE',  ( -16.17053951239850207, 32.72994544565565889, -6.425226171708652956 ) ) ;
#9586 = ADVANCED_FACE ( 'NONE', ( #9226 ), #7904, .F. ) ;
#9587 = ORIENTED_EDGE ( 'NONE', *, *, #6528, .F. ) ;
#9588 = EDGE_CURVE ( 'NONE', #1561, #16968, #12237, .T. ) ;
#9589 = ORIENTED_EDGE ( 'NONE', *, *, #11641, .T. ) ;
#9590 = CARTESIAN_POINT ( 'NONE',  ( -187.6513770290094385, 173.0877615073859772, -1.855974361197849420 ) ) ;
#9591 = CARTESIAN_POINT ( 'NONE',  ( 8.038468667238035437, 139.4170824625289242, 14.76281475457819070 ) ) ;
#9592 = CIRCLE ( 'NONE', #5931, 35.00000000000000000 ) ;
#9593 = VERTEX_POINT ( 'NONE', #16321 ) ;
#9594 = VECTOR ( 'NONE', #6569, 1000.000000000000000 ) ;
#9595 = FACE_OUTER_BOUND ( 'NONE', #6008, .T. ) ;
#9596 = VECTOR ( 'NONE', #15404, 1000.000000000000114 ) ;
#9597 = DIRECTION ( 'NONE',  ( 1.000000000000000000, 1.156482317317868274E-16, -0.000000000000000000 ) ) ;
#9598 = CARTESIAN_POINT ( 'NONE',  ( -725.0000000000000000, 19.99999999999995737, 4.999999999999999112 ) ) ;
#9599 = DIRECTION ( 'NONE',  ( -0.000000000000000000, -0.000000000000000000, 1.000000000000000000 ) ) ;
#9600 = CARTESIAN_POINT ( 'NONE',  ( -82.41118593285520433, 151.0069623973649868, 25.76819119792229529 ) ) ;
#9601 = ORIENTED_EDGE ( 'NONE', *, *, #15270, .F. ) ;
#9602 = CARTESIAN_POINT ( 'NONE',  ( -76.84835529096334028, 201.7321575960915538, -17.84571802696395082 ) ) ;
#9603 = CARTESIAN_POINT ( 'NONE',  ( -82.50000000000001421, 196.6227766016838245, 0.000000000000000000 ) ) ;
#9604 = CARTESIAN_POINT ( 'NONE',  ( 17.00000000000000000, 171.6227766016838245, 20.00000000000000355 ) ) ;
#9605 = DIRECTION ( 'NONE',  ( 0.000000000000000000, 0.000000000000000000, -1.000000000000000000 ) ) ;
#9606 = CARTESIAN_POINT ( 'NONE',  ( -95.00000000000000000, 171.6227766016838245, 27.69059892324149530 ) ) ;
#9607 = VECTOR ( 'NONE', #13426, 1000.000000000000000 ) ;
#9608 = AXIS2_PLACEMENT_3D ( 'NONE', #1593, #6994, #8306 ) ;
#9609 = VERTEX_POINT ( 'NONE', #4190 ) ;
#9610 = AXIS2_PLACEMENT_3D ( 'NONE', #5216, #14515, #16023 ) ;
#9611 = DIRECTION ( 'NONE',  ( 1.000000000000000000, -0.000000000000000000, -0.000000000000000000 ) ) ;
#9612 = ORIENTED_EDGE ( 'NONE', *, *, #2520, .T. ) ;
#9613 = FACE_OUTER_BOUND ( 'NONE', #15821, .T. ) ;
#9614 = EDGE_LOOP ( 'NONE', ( #13350, #2686 ) ) ;
#9615 = FILL_AREA_STYLE ('',( #4137 ) ) ;
#9616 = DIRECTION ( 'NONE',  ( -1.000000000000000000, -6.938893903907228378E-16, 0.000000000000000000 ) ) ;
#9617 = DIRECTION ( 'NONE',  ( 0.000000000000000000, 0.000000000000000000, 1.000000000000000000 ) ) ;
#9618 = DIRECTION ( 'NONE',  ( -1.337133840571206485E-16, 0.000000000000000000, -1.000000000000000000 ) ) ;
#9619 = AXIS2_PLACEMENT_3D ( 'NONE', #2626, #14662, #8097 ) ;
#9620 = VECTOR ( 'NONE', #6162, 1000.000000000000000 ) ;
#9621 = EDGE_LOOP ( 'NONE', ( #9001, #7231 ) ) ;
#9622 = DIRECTION ( 'NONE',  ( 0.000000000000000000, 0.000000000000000000, 1.000000000000000000 ) ) ;
#9623 = CARTESIAN_POINT ( 'NONE',  ( 1.559999999999998943, -1.732050807568885631, 0.000000000000000000 ) ) ;
#9624 = CARTESIAN_POINT ( 'NONE',  ( -80.00000000000001421, 196.6227766016838245, -35.00200000000000244 ) ) ;
#9625 = EDGE_CURVE ( 'NONE', #1652, #374, #11973, .T. ) ;
#9626 = DIRECTION ( 'NONE',  ( -1.000000000000000000, 0.000000000000000000, 0.000000000000000000 ) ) ;
#9627 = CARTESIAN_POINT ( 'NONE',  ( 26.85584576128377066, 137.3904121345421458, -7.294850950184896377 ) ) ;
#9628 = ORIENTED_EDGE ( 'NONE', *, *, #8104, .F. ) ;
#9629 = PLANE ( 'NONE',  #8386 ) ;
#9630 = DIRECTION ( 'NONE',  ( 1.337133840571206485E-16, 0.000000000000000000, -1.000000000000000000 ) ) ;
#9631 = ORIENTED_EDGE ( 'NONE', *, *, #11933, .F. ) ;
#9632 = CARTESIAN_POINT ( 'NONE',  ( 0.000000000000000000, 0.000000000000000000, 0.000000000000000000 ) ) ;
#9633 = CARTESIAN_POINT ( 'NONE',  ( -50.00000000000000000, 171.6227766016838245, 0.000000000000000000 ) ) ;
#9634 = DIRECTION ( 'NONE',  ( -0.000000000000000000, -0.000000000000000000, 1.000000000000000000 ) ) ;
#9635 = CARTESIAN_POINT ( 'NONE',  ( 30.20512376220668926, 191.6231342001797202, 26.24853702829030766 ) ) ;
#9636 = CARTESIAN_POINT ( 'NONE',  ( 0.000000000000000000, 0.8660254037844428154, 1.500000000000001332 ) ) ;
#9637 = CARTESIAN_POINT ( 'NONE',  ( 48.00000000000000711, 187.6227766016837961, -12.50000337241049309 ) ) ;
#9638 = CIRCLE ( 'NONE', #12484, 5.000000000000007994 ) ;
#9639 = DIRECTION ( 'NONE',  ( -1.000000000000000000, 0.000000000000000000, 0.000000000000000000 ) ) ;
#9640 = DIRECTION ( 'NONE',  ( 0.000000000000000000, 0.000000000000000000, 1.000000000000000000 ) ) ;
#9641 = ADVANCED_FACE ( 'NONE', ( #13313 ), #1178, .F. ) ;
#9642 = CARTESIAN_POINT ( 'NONE',  ( 1.559999999999998943, 0.8660254037844428154, 1.500000000000001332 ) ) ;
#9643 = ORIENTED_EDGE ( 'NONE', *, *, #3823, .F. ) ;
#9644 = CARTESIAN_POINT ( 'NONE',  ( -11.18069906337402664, 30.84474844633047397, -14.38199110044527274 ) ) ;
#9645 = ORIENTED_EDGE ( 'NONE', *, *, #15326, .F. ) ;
#9646 = CARTESIAN_POINT ( 'NONE',  ( 24.67949051125555826, 29.87169671703155771, -7.269639412668861489 ) ) ;
#9647 = ADVANCED_FACE ( 'NONE', ( #12584 ), #449, .F. ) ;
#9648 = DIRECTION ( 'NONE',  ( -0.000000000000000000, -0.000000000000000000, -1.000000000000000000 ) ) ;
#9649 = ORIENTED_EDGE ( 'NONE', *, *, #7974, .F. ) ;
#9650 = ADVANCED_FACE ( 'NONE', ( #7182 ), #11348, .F. ) ;
#9651 = CARTESIAN_POINT ( 'NONE',  ( -23.66837786580496328, 19.99999999999999645, 17.32703391567687135 ) ) ;
#9652 = EDGE_CURVE ( 'NONE', #4393, #6638, #3290, .T. ) ;
#9653 = LINE ( 'NONE', #1516, #17210 ) ;
#9654 = ORIENTED_EDGE ( 'NONE', *, *, #2970, .F. ) ;
#9655 = CARTESIAN_POINT ( 'NONE',  ( 33.81731182140757852, 153.1022248993912171, -27.31438289289431864 ) ) ;
#9656 = VERTEX_POINT ( 'NONE', #8517 ) ;
#9657 = CARTESIAN_POINT ( 'NONE',  ( 27.30499999999999616, 0.000000000000000000, 0.000000000000000000 ) ) ;
#9658 = DIRECTION ( 'NONE',  ( 0.000000000000000000, 0.000000000000000000, 1.000000000000000000 ) ) ;
#9659 = CARTESIAN_POINT ( 'NONE',  ( 17.00000000000000000, 191.6227766016837961, -1.224646799147353454E-15 ) ) ;
#9660 = EDGE_LOOP ( 'NONE', ( #4264, #13055, #9143, #5629 ) ) ;
#9661 = DIRECTION ( 'NONE',  ( 0.000000000000000000, -8.673617379884035472E-17, 1.000000000000000000 ) ) ;
#9662 = CARTESIAN_POINT ( 'NONE',  ( -45.00000000000000000, 122.0000000000000142, 4.999999999999999112 ) ) ;
#9663 = ORIENTED_EDGE ( 'NONE', *, *, #8135, .T. ) ;
#9664 = DIRECTION ( 'NONE',  ( 0.000000000000000000, 0.000000000000000000, 1.000000000000000000 ) ) ;
#9665 = ORIENTED_EDGE ( 'NONE', *, *, #9160, .T. ) ;
#9666 = CARTESIAN_POINT ( 'NONE',  ( -86.08081429761091385, 192.2260612991243534, -25.77925661938086677 ) ) ;
#9667 = LINE ( 'NONE', #15153, #12621 ) ;
#9668 = DIRECTION ( 'NONE',  ( 0.000000000000000000, -1.000000000000000000, -0.000000000000000000 ) ) ;
#9669 = ORIENTED_EDGE ( 'NONE', *, *, #3638, .T. ) ;
#9670 = EDGE_LOOP ( 'NONE', ( #11220, #5037, #3344, #4498, #13303 ) ) ;
#9671 = DIRECTION ( 'NONE',  ( 0.000000000000000000, 0.000000000000000000, 1.000000000000000000 ) ) ;
#9672 = CARTESIAN_POINT ( 'NONE',  ( -72.94847233519770668, 199.2234891967518422, -18.10843944793621674 ) ) ;
#9673 = CARTESIAN_POINT ( 'NONE',  ( 6.134011831684059501, 142.5209969267753820, 19.44444444444444642 ) ) ;
#9674 = EDGE_LOOP ( 'NONE', ( #17183, #11314, #16308, #1840, #4734, #10382 ) ) ;
#9675 = SHAPE_DEFINITION_REPRESENTATION ( #1930, #5345 ) ;
#9676 = CARTESIAN_POINT ( 'NONE',  ( -45.00000000000000000, 142.5209969267753820, 19.44444444444444997 ) ) ;
#9677 = FACE_OUTER_BOUND ( 'NONE', #8082, .T. ) ;
#9678 = DIRECTION ( 'NONE',  ( -1.000000000000000000, 0.000000000000000000, 0.000000000000000000 ) ) ;
#9679 = ADVANCED_FACE ( 'NONE', ( #5858 ), #12321, .F. ) ;
#9680 = DIRECTION ( 'NONE',  ( -1.000000000000000000, 0.000000000000000000, 0.000000000000000000 ) ) ;
#9681 = EDGE_CURVE ( 'NONE', #2477, #3947, #288, .T. ) ;
#9682 = CARTESIAN_POINT ( 'NONE',  ( 19.87492423018547427, 17.99999999999543121, 11.43634947295695703 ) ) ;
#9683 = PRODUCT_DEFINITION_SHAPE ( 'NONE', 'NONE',  #49 ) ;
#9684 = ORIENTED_EDGE ( 'NONE', *, *, #1233, .F. ) ;
#9685 = CARTESIAN_POINT ( 'NONE',  ( -86.00000000000004263, 196.8086972563010022, -24.30514295430833371 ) ) ;
#9686 = CARTESIAN_POINT ( 'NONE',  ( -2.428612866367531510E-15, 2.000000000000000000, -28.00000000000000711 ) ) ;
#9687 = CARTESIAN_POINT ( 'NONE',  ( -100.0000000000000000, 171.6227766016838245, 0.000000000000000000 ) ) ;
#9688 = DIRECTION ( 'NONE',  ( -1.000000000000000000, -6.938893903907228378E-16, -0.000000000000000000 ) ) ;
#9689 = CYLINDRICAL_SURFACE ( 'NONE', #10060, 5.000000000000018652 ) ;
#9690 = ORIENTED_EDGE ( 'NONE', *, *, #1859, .F. ) ;
#9691 = VERTEX_POINT ( 'NONE', #16672 ) ;
#9692 = CARTESIAN_POINT ( 'NONE',  ( -15.00000000000002132, 100.0000000000000142, -4.999999999999999112 ) ) ;
#9693 = EDGE_LOOP ( 'NONE', ( #10222, #4745 ) ) ;
#9694 = CYLINDRICAL_SURFACE ( 'NONE', #9530, 2.500000000000000444 ) ;
#9695 = VERTEX_POINT ( 'NONE', #8328 ) ;
#9696 = PRESENTATION_STYLE_ASSIGNMENT (( #16187 ) ) ;
#9697 = LINE ( 'NONE', #13693, #3691 ) ;
#9698 = DIRECTION ( 'NONE',  ( -1.000000000000000000, -0.000000000000000000, 0.000000000000000000 ) ) ;
#9699 = DIRECTION ( 'NONE',  ( 1.000000000000000000, -0.000000000000000000, -0.000000000000000000 ) ) ;
#9700 = EDGE_CURVE ( 'NONE', #1100, #7826, #13741, .T. ) ;
#9701 = EDGE_CURVE ( 'NONE', #17135, #313, #3158, .T. ) ;
#9702 = CARTESIAN_POINT ( 'NONE',  ( -206.3689767832464668, 174.5534660175772785, -3.987129972734268168 ) ) ;
#9703 = ADVANCED_FACE ( 'NONE', ( #4542 ), #5690, .T. ) ;
#9704 = UNCERTAINTY_MEASURE_WITH_UNIT (LENGTH_MEASURE( 1.000000000000000082E-05 ), #12385, 'distance_accuracy_value', 'NONE');
#9705 = EDGE_CURVE ( 'NONE', #216, #6230, #15330, .T. ) ;
#9706 = ORIENTED_EDGE ( 'NONE', *, *, #7461, .T. ) ;
#9707 = CARTESIAN_POINT ( 'NONE',  ( -100.0000000000000000, 171.6227766016838245, 0.000000000000000000 ) ) ;
#9708 = DIRECTION ( 'NONE',  ( -0.000000000000000000, -0.000000000000000000, -1.000000000000000000 ) ) ;
#9709 = CARTESIAN_POINT ( 'NONE',  ( -31.89848094669886436, 119.9728602285818084, 5.500000000000000000 ) ) ;
#9710 = B_SPLINE_CURVE_WITH_KNOTS ( 'NONE', 3,
 ( #7298, #16864, #13774, #5980, #11372, #4735, #8358, #13871, #1644, #314 ),
 .UNSPECIFIED., .F., .F.,
 ( 4, 2, 2, 2, 4 ),
 ( 0.0003067249959486805411, 0.0007024845516937958632, 0.001098244107438911240, 0.001494003663184026399, 0.001889763218929141775 ),
 .UNSPECIFIED. ) ;
#9711 = CARTESIAN_POINT ( 'NONE',  ( -98.00000000000000000, 171.6227766016838245, 0.000000000000000000 ) ) ;
#9712 = CARTESIAN_POINT ( 'NONE',  ( 14.91849273675205545, 128.9263856399286396, -11.14803070335530855 ) ) ;
#9713 = ORIENTED_EDGE ( 'NONE', *, *, #16742, .T. ) ;
#9714 = FACE_BOUND ( 'NONE', #2117, .T. ) ;
#9715 = CARTESIAN_POINT ( 'NONE',  ( 26.76721132277178228, 139.3994271089711958, -7.121518580654788266 ) ) ;
#9716 = ORIENTED_EDGE ( 'NONE', *, *, #7208, .F. ) ;
#9717 =( NAMED_UNIT ( * ) SI_UNIT ( $, .STERADIAN. ) SOLID_ANGLE_UNIT ( ) );
#9718 = CYLINDRICAL_SURFACE ( 'NONE', #1135, 12.00000000000000000 ) ;
#9719 = EDGE_CURVE ( 'NONE', #12351, #5017, #15143, .T. ) ;
#9720 = CARTESIAN_POINT ( 'NONE',  ( 196.0000000000000000, 179.6227766016838245, 12.50000337241049309 ) ) ;
#9721 = CARTESIAN_POINT ( 'NONE',  ( 28.46817412490414512, 191.8593874686152674, 26.06696055488264108 ) ) ;
#9722 = CARTESIAN_POINT ( 'NONE',  ( 25.49999999999998579, 9.999999999999998224, -16.00000000000000000 ) ) ;
#9723 = SHAPE_REPRESENTATION ( 'BR-801', ( #7002, #5861, #6139, #775, #9517, #11777, #6714, #4161, #16616, #8959, #14065, #505, #10676, #14353, #12369, #13798 ), #10384 ) ;
#9724 = LINE ( 'NONE', #16473, #198 ) ;
#9725 = CARTESIAN_POINT ( 'NONE',  ( 18.00561851734427421, 29.93835620586352064, 12.40035566057732375 ) ) ;
#9726 = CARTESIAN_POINT ( 'NONE',  ( -83.43806183198967119, 200.2660383695261714, 16.39286986631257292 ) ) ;
#9727 = DIRECTION ( 'NONE',  ( 1.000000000000000000, 0.000000000000000000, 0.000000000000000000 ) ) ;
#9728 = VECTOR ( 'NONE', #15217, 1000.000000000000000 ) ;
#9729 = VERTEX_POINT ( 'NONE', #11078 ) ;
#9730 = VERTEX_POINT ( 'NONE', #12501 ) ;
#9731 = CARTESIAN_POINT ( 'NONE',  ( -75.00000000000000000, 196.6227766016838245, 0.000000000000000000 ) ) ;
#9732 = DIRECTION ( 'NONE',  ( 0.000000000000000000, 0.000000000000000000, 1.000000000000000000 ) ) ;
#9733 = VERTEX_POINT ( 'NONE', #10992 ) ;
#9734 = CARTESIAN_POINT ( 'NONE',  ( -102.0000000000000142, 171.6227766016838245, 0.000000000000000000 ) ) ;
#9735 = CARTESIAN_POINT ( 'NONE',  ( -95.00000000000000000, 171.6227766016838245, -30.00000000000000000 ) ) ;
#9736 = VERTEX_POINT ( 'NONE', #9659 ) ;
#9737 = EDGE_CURVE ( 'NONE', #4814, #730, #12677, .T. ) ;
#9738 = CARTESIAN_POINT ( 'NONE',  ( 22.50701606102701646, 147.0010062438373382, -21.97388680505720515 ) ) ;
#9739 = ADVANCED_FACE ( 'NONE', ( #4450 ), #8424, .F. ) ;
#9740 = AXIS2_PLACEMENT_3D ( 'NONE', #9404, #16494, #16233 ) ;
#9741 = DIRECTION ( 'NONE',  ( -1.000000000000000000, 0.000000000000000000, 0.000000000000000000 ) ) ;
#9742 = CIRCLE ( 'NONE', #5794, 12.00000000000000000 ) ;
#9743 = DIRECTION ( 'NONE',  ( -1.000000000000000000, 0.000000000000000000, 0.000000000000000000 ) ) ;
#9744 = CARTESIAN_POINT ( 'NONE',  ( 1.559999999999998943, -1.732050807568885631, 0.000000000000000000 ) ) ;
#9745 = DIRECTION ( 'NONE',  ( 0.000000000000000000, 0.000000000000000000, 1.000000000000000000 ) ) ;
#9746 = CARTESIAN_POINT ( 'NONE',  ( 0.000000000000000000, -0.8660254037844428154, -1.499999999999997780 ) ) ;
#9747 = EDGE_CURVE ( 'NONE', #15915, #11290, #6918, .T. ) ;
#9748 = ADVANCED_FACE ( 'NONE', ( #3117 ), #1366, .T. ) ;
#9749 = CARTESIAN_POINT ( 'NONE',  ( 17.00000000000000000, 171.6227766016838245, -20.00000000000000355 ) ) ;
#9750 = EDGE_LOOP ( 'NONE', ( #16334, #468 ) ) ;
#9751 = DIRECTION ( 'NONE',  ( 0.000000000000000000, 0.000000000000000000, -1.000000000000000000 ) ) ;
#9752 = ADVANCED_FACE ( 'NONE', ( #6738 ), #2389, .T. ) ;
#9753 = ORIENTED_EDGE ( 'NONE', *, *, #10259, .F. ) ;
#9754 = DIRECTION ( 'NONE',  ( 8.673617379884037937E-17, 0.000000000000000000, -1.000000000000000000 ) ) ;
#9755 = CARTESIAN_POINT ( 'NONE',  ( -95.00000000000000000, 171.6227766016838245, 0.000000000000000000 ) ) ;
#9756 = AXIS2_PLACEMENT_3D ( 'NONE', #11157, #7181, #550 ) ;
#9757 = CARTESIAN_POINT ( 'NONE',  ( 25.00000000000000711, 146.6227766016838245, 35.00200000000000244 ) ) ;
#9758 = AXIS2_PLACEMENT_3D ( 'NONE', #15314, #14084, #4521 ) ;
#9759 = EDGE_LOOP ( 'NONE', ( #15463, #2464 ) ) ;
#9760 = ORIENTED_EDGE ( 'NONE', *, *, #1758, .F. ) ;
#9761 = DIRECTION ( 'NONE',  ( 1.000000000000000000, 0.000000000000000000, 0.000000000000000000 ) ) ;
#9762 = AXIS2_PLACEMENT_3D ( 'NONE', #4090, #6748, #12048 ) ;
#9763 = CARTESIAN_POINT ( 'NONE',  ( 15.96677753506825681, 136.6227766017765930, 1.239574023933039948 ) ) ;
#9764 = CARTESIAN_POINT ( 'NONE',  ( 26.76721132277178228, 137.4464968366854407, 7.553125767360616472 ) ) ;
#9765 = EDGE_LOOP ( 'NONE', ( #2286, #16203, #7344 ) ) ;
#9766 = PRODUCT_CONTEXT ( 'NONE', #4617, 'mechanical' ) ;
#9767 = DIRECTION ( 'NONE',  ( 0.000000000000000000, 0.000000000000000000, 1.000000000000000000 ) ) ;
#9768 = DIRECTION ( 'NONE',  ( -1.000000000000000000, 0.000000000000000000, 0.000000000000000000 ) ) ;
#9769 = FACE_OUTER_BOUND ( 'NONE', #3128, .T. ) ;
#9770 = CARTESIAN_POINT ( 'NONE',  ( -34.99999999999999289, 120.0000000000000000, 0.000000000000000000 ) ) ;
#9771 = CARTESIAN_POINT ( 'NONE',  ( 17.13110662433428288, 29.95577564710725227, 12.69327266642979168 ) ) ;
#9772 = AXIS2_PLACEMENT_3D ( 'NONE', #8901, #6333, #11726 ) ;
#9773 = LINE ( 'NONE', #69, #4085 ) ;
#9774 = ADVANCED_FACE ( 'NONE', ( #6648 ), #11952, .T. ) ;
#9775 = ORIENTED_EDGE ( 'NONE', *, *, #3798, .F. ) ;
#9776 = DIRECTION ( 'NONE',  ( -1.000000000000000000, 0.000000000000000000, 0.000000000000000000 ) ) ;
#9777 = DIRECTION ( 'NONE',  ( 0.000000000000000000, 0.8660254037844380415, -0.5000000000000012212 ) ) ;
#9778 = DIRECTION ( 'NONE',  ( 0.000000000000000000, 1.000000000000000000, 0.000000000000000000 ) ) ;
#9779 = DIRECTION ( 'NONE',  ( -0.000000000000000000, 1.000000000000000000, -0.000000000000000000 ) ) ;
#9780 = DIRECTION ( 'NONE',  ( 0.000000000000000000, -1.000000000000000000, -6.123233995736762338E-17 ) ) ;
#9781 = EDGE_LOOP ( 'NONE', ( #9830, #5763, #7645, #16141, #17144, #3647, #4123 ) ) ;
#9782 = ORIENTED_EDGE ( 'NONE', *, *, #15742, .F. ) ;
#9783 = CLOSED_SHELL ( 'NONE', ( #8885, #9235, #5638, #10274, #3476, #17019, #8604, #16849, #12631, #1214, #13022, #782 ) ) ;
#9784 = AXIS2_PLACEMENT_3D ( 'NONE', #6051, #8616, #3482 ) ;
#9785 = DIRECTION ( 'NONE',  ( -1.000000000000000000, -0.000000000000000000, -0.000000000000000000 ) ) ;
#9786 = ADVANCED_FACE ( 'NONE', ( #17354 ), #2484, .F. ) ;
#9787 = VECTOR ( 'NONE', #9582, 1000.000000000000000 ) ;
#9788 = ORIENTED_EDGE ( 'NONE', *, *, #2294, .F. ) ;
#9789 =( NAMED_UNIT ( * ) SI_UNIT ( $, .STERADIAN. ) SOLID_ANGLE_UNIT ( ) );
#9790 = ORIENTED_EDGE ( 'NONE', *, *, #7490, .T. ) ;
#9791 = SHAPE_REPRESENTATION_RELATIONSHIP ( 'NONE' , 'NONE' ,  #17442, #16081 ) ;
#9792 = CARTESIAN_POINT ( 'NONE',  ( -22.99999999999999289, 90.00000000000000000, 4.999999999999999112 ) ) ;
#9793 = DIRECTION ( 'NONE',  ( 1.000000000000000000, -0.000000000000000000, -0.000000000000000000 ) ) ;
#9794 = LINE ( 'NONE', #15194, #14854 ) ;
#9795 = VECTOR ( 'NONE', #712, 1000.000000000000000 ) ;
#9796 = AXIS2_PLACEMENT_3D ( 'NONE', #12935, #1154, #7781 ) ;
#9797 = VERTEX_POINT ( 'NONE', #3910 ) ;
#9798 = CARTESIAN_POINT ( 'NONE',  ( 50.00000000000000000, 171.6227766016838245, 0.000000000000000000 ) ) ;
#9799 = CARTESIAN_POINT ( 'NONE',  ( -153.0000000000000284, 171.6227766016838245, 0.000000000000000000 ) ) ;
#9800 = VECTOR ( 'NONE', #169, 1000.000000000000000 ) ;
#9801 = CARTESIAN_POINT ( 'NONE',  ( 196.0000000000000000, 179.6227766016838245, 12.50000337241049309 ) ) ;
#9802 = COLOUR_RGB ( '', 0.09019608, 0.27058824, 0.51372549) ;
#9803 = FACE_OUTER_BOUND ( 'NONE', #8262, .T. ) ;
#9804 = AXIS2_PLACEMENT_3D ( 'NONE', #9895, #11573, #1934 ) ;
#9805 = DIRECTION ( 'NONE',  ( -0.000000000000000000, -0.000000000000000000, -1.000000000000000000 ) ) ;
#9806 = ADVANCED_FACE ( 'NONE', ( #13291 ), #10622, .T. ) ;
#9807 = ADVANCED_FACE ( 'NONE', ( #9386 ), #1428, .T. ) ;
#9808 = EDGE_CURVE ( 'NONE', #13439, #735, #4224, .T. ) ;
#9809 = ORIENTED_EDGE ( 'NONE', *, *, #11106, .T. ) ;
#9810 = CYLINDRICAL_SURFACE ( 'NONE', #17152, 7.499999999999996447 ) ;
#9811 = ORIENTED_EDGE ( 'NONE', *, *, #13086, .T. ) ;
#9812 = CARTESIAN_POINT ( 'NONE',  ( -100.0000000000000000, 134.2062027339443944, -25.00000000000000000 ) ) ;
#9813 = CIRCLE ( 'NONE', #15471, 20.00000000000000355 ) ;
#9814 = DIRECTION ( 'NONE',  ( -1.000000000000000000, 0.000000000000000000, 0.000000000000000000 ) ) ;
#9815 = LINE ( 'NONE', #12559, #9800 ) ;
#9816 = LINE ( 'NONE', #11326, #15952 ) ;
#9817 = CARTESIAN_POINT ( 'NONE',  ( 27.99999999999998224, 9.999999999999998224, -16.00000000000000000 ) ) ;
#9818 = DIRECTION ( 'NONE',  ( -1.000000000000000000, -0.000000000000000000, 0.000000000000000000 ) ) ;
#9819 = LINE ( 'NONE', #2033, #7916 ) ;
#9820 = CARTESIAN_POINT ( 'NONE',  ( 20.49999999999998224, 10.00000000000000000, -13.00000000000000000 ) ) ;
#9821 = ORIENTED_EDGE ( 'NONE', *, *, #13803, .T. ) ;
#9822 = ORIENTED_EDGE ( 'NONE', *, *, #10501, .T. ) ;
#9823 = CARTESIAN_POINT ( 'NONE',  ( 24.93507336697353338, 29.86842105263157521, -5.000000000000004441 ) ) ;
#9824 = AXIS2_PLACEMENT_3D ( 'NONE', #1234, #5405, #16207 ) ;
#9825 = FACE_OUTER_BOUND ( 'NONE', #16206, .T. ) ;
#9826 = ORIENTED_EDGE ( 'NONE', *, *, #3062, .F. ) ;
#9827 = CARTESIAN_POINT ( 'NONE',  ( -18.18164784767110120, 32.29378831700660157, 6.323624269675778287 ) ) ;
#9828 = ADVANCED_FACE ( 'NONE', ( #5322 ), #14707, .T. ) ;
#9829 = DIRECTION ( 'NONE',  ( 0.000000000000000000, 0.000000000000000000, -1.000000000000000000 ) ) ;
#9830 = ORIENTED_EDGE ( 'NONE', *, *, #15036, .F. ) ;
#9831 = CARTESIAN_POINT ( 'NONE',  ( 37.47214505283547936, 147.3844239155462503, -22.40167687543584663 ) ) ;
#9832 =( BOUNDED_CURVE ( )  B_SPLINE_CURVE ( 3, ( #7852, #11739, #10780, #17241 ),
 .UNSPECIFIED., .F., .F. ) 
 B_SPLINE_CURVE_WITH_KNOTS ( ( 4, 4 ),
 ( 4.712388980384692339, 6.283185307179586232 ),
 .UNSPECIFIED. ) 
 CURVE ( )  GEOMETRIC_REPRESENTATION_ITEM ( )  RATIONAL_B_SPLINE_CURVE ( ( 1.000000000000000000, 0.8047378541243654926, 0.8047378541243654926, 1.000000000000000000 ) ) 
 REPRESENTATION_ITEM ( '' )  );
#9833 = CARTESIAN_POINT ( 'NONE',  ( -19.79962810613639945, 18.00000000000000711, 20.97942696524416206 ) ) ;
#9834 = AXIS2_PLACEMENT_3D ( 'NONE', #3573, #2246, #11794 ) ;
#9835 = AXIS2_PLACEMENT_3D ( 'NONE', #6641, #13368, #12037 ) ;
#9836 = DIRECTION ( 'NONE',  ( 0.000000000000000000, -1.000000000000000000, 0.000000000000000000 ) ) ;
#9837 =( GEOMETRIC_REPRESENTATION_CONTEXT ( 3 ) GLOBAL_UNCERTAINTY_ASSIGNED_CONTEXT ( ( #16009 ) ) GLOBAL_UNIT_ASSIGNED_CONTEXT ( ( #6009, #12998, #3179 ) ) REPRESENTATION_CONTEXT ( 'NONE', 'WORKASPACE' ) );
#9838 = CARTESIAN_POINT ( 'NONE',  ( -68.00000000000000000, 154.3022685259950038, 9.999999999999900524 ) ) ;
#9839 = DIRECTION ( 'NONE',  ( -1.000000000000000000, -0.000000000000000000, -0.000000000000000000 ) ) ;
#9840 = LINE ( 'NONE', #11159, #6073 ) ;
#9841 = CARTESIAN_POINT ( 'NONE',  ( 30.00000000000000355, 196.6227766016838245, -12.99999999999999822 ) ) ;
#9842 = ORIENTED_EDGE ( 'NONE', *, *, #10337, .F. ) ;
#9843 = CARTESIAN_POINT ( 'NONE',  ( 11.02544963116560517, 142.2295695439714791, -19.00161275228506952 ) ) ;
#9844 = ORIENTED_EDGE ( 'NONE', *, *, #15009, .F. ) ;
#9845 = EDGE_CURVE ( 'NONE', #14060, #15553, #6469, .T. ) ;
#9846 = CARTESIAN_POINT ( 'NONE',  ( 49.99999999999998579, 179.6227766016838245, -10.00000337241049309 ) ) ;
#9847 = DIRECTION ( 'NONE',  ( 1.000000000000000000, 0.000000000000000000, 0.000000000000000000 ) ) ;
#9848 = AXIS2_PLACEMENT_3D ( 'NONE', #5773, #11082, #4547 ) ;
#9849 = ORIENTED_EDGE ( 'NONE', *, *, #5496, .T. ) ;
#9850 = ORIENTED_EDGE ( 'NONE', *, *, #4565, .F. ) ;
#9851 = CARTESIAN_POINT ( 'NONE',  ( -24.99999999999999645, 120.0000000000000284, 4.999999999999999112 ) ) ;
#9852 = CIRCLE ( 'NONE', #11266, 2.500000000000000444 ) ;
#9853 = CARTESIAN_POINT ( 'NONE',  ( 15.93460003626534238, 136.8193095811534761, 3.708327557688629206 ) ) ;
#9854 = CARTESIAN_POINT ( 'NONE',  ( 15.51497662817079082, 137.3737080369936905, 9.118346648348486738 ) ) ;
#9855 = ORIENTED_EDGE ( 'NONE', *, *, #4925, .F. ) ;
#9856 = CARTESIAN_POINT ( 'NONE',  ( -100.0000000000000000, 143.0439382767972347, 16.49999999999984368 ) ) ;
#9857 = DIRECTION ( 'NONE',  ( 1.000000000000000000, 0.000000000000000000, 0.000000000000000000 ) ) ;
#9858 = CARTESIAN_POINT ( 'NONE',  ( -84.64903570047881942, 194.7608640721562381, 23.53240337055842701 ) ) ;
#9859 = LINE ( 'NONE', #11278, #15868 ) ;
#9860 = CARTESIAN_POINT ( 'NONE',  ( 18.23439605415255471, 29.93382634594462743, 12.29196570735054728 ) ) ;
#9861 = VECTOR ( 'NONE', #9779, 1000.000000000000000 ) ;
#9862 = DIRECTION ( 'NONE',  ( 1.000000000000000000, 0.000000000000000000, 0.000000000000000000 ) ) ;
#9863 = CIRCLE ( 'NONE', #12409, 11.99999999999999645 ) ;
#9864 = ORIENTED_EDGE ( 'NONE', *, *, #1457, .F. ) ;
#9865 = CARTESIAN_POINT ( 'NONE',  ( -76.36507656924925413, 201.4000939832746724, -18.39459910103776963 ) ) ;
#9866 = LINE ( 'NONE', #3148, #6815 ) ;
#9867 = DIRECTION ( 'NONE',  ( -1.000000000000000000, -0.000000000000000000, -0.000000000000000000 ) ) ;
#9868 = EDGE_CURVE ( 'NONE', #2736, #8582, #2661, .T. ) ;
#9869 = DIRECTION ( 'NONE',  ( -1.000000000000000000, 0.000000000000000000, 0.000000000000000000 ) ) ;
#9870 = DIRECTION ( 'NONE',  ( -1.000000000000000000, 0.000000000000000000, 0.000000000000000000 ) ) ;
#9871 = ORIENTED_EDGE ( 'NONE', *, *, #15837, .F. ) ;
#9872 = VERTEX_POINT ( 'NONE', #1067 ) ;
#9873 = AXIS2_PLACEMENT_3D ( 'NONE', #5471, #246, #9534 ) ;
#9874 = EDGE_CURVE ( 'NONE', #12401, #14513, #10710, .T. ) ;
#9875 = CARTESIAN_POINT ( 'NONE',  ( 12.56741672263938625, 143.7071609262609400, 17.59902447249972113 ) ) ;
#9876 = AXIS2_PLACEMENT_3D ( 'NONE', #459, #7375, #13851 ) ;
#9877 = ORIENTED_EDGE ( 'NONE', *, *, #6677, .F. ) ;
#9878 = EDGE_CURVE ( 'NONE', #7262, #6472, #12697, .T. ) ;
#9879 = DIRECTION ( 'NONE',  ( -1.000000000000000000, 0.000000000000000000, 0.000000000000000000 ) ) ;
#9880 = AXIS2_PLACEMENT_3D ( 'NONE', #872, #13163, #10319 ) ;
#9881 = EDGE_CURVE ( 'NONE', #16273, #190, #8053, .T. ) ;
#9882 = ORIENTED_EDGE ( 'NONE', *, *, #8299, .F. ) ;
#9883 = CYLINDRICAL_SURFACE ( 'NONE', #13020, 5.000000000000000888 ) ;
#9884 =( NAMED_UNIT ( * ) SI_UNIT ( $, .STERADIAN. ) SOLID_ANGLE_UNIT ( ) );
#9885 = DIRECTION ( 'NONE',  ( 0.000000000000000000, 0.000000000000000000, -1.000000000000000000 ) ) ;
#9886 = CARTESIAN_POINT ( 'NONE',  ( 225.0000000000000000, 89.99999999999997158, 15.00000000000000000 ) ) ;
#9887 = ORIENTED_EDGE ( 'NONE', *, *, #3616, .T. ) ;
#9888 = DIRECTION ( 'NONE',  ( -1.000000000000000000, -0.000000000000000000, 0.000000000000000000 ) ) ;
#9889 = CIRCLE ( 'NONE', #9316, 27.69059892324149530 ) ;
#9890 = PLANE ( 'NONE',  #14136 ) ;
#9891 = EDGE_CURVE ( 'NONE', #15022, #13094, #8745, .T. ) ;
#9892 = LINE ( 'NONE', #2984, #6223 ) ;
#9893 = FACE_OUTER_BOUND ( 'NONE', #11821, .T. ) ;
#9894 = ORIENTED_EDGE ( 'NONE', *, *, #1598, .T. ) ;
#9895 = CARTESIAN_POINT ( 'NONE',  ( 30.00000000000001066, 146.6227766016838245, 10.00000000000000178 ) ) ;
#9896 = AXIS2_PLACEMENT_3D ( 'NONE', #12103, #15091, #17410 ) ;
#9897 = AXIS2_PLACEMENT_3D ( 'NONE', #5913, #11308, #16723 ) ;
#9898 = VERTEX_POINT ( 'NONE', #5414 ) ;
#9899 = SURFACE_STYLE_USAGE ( .BOTH. , #15213 ) ;
#9900 = CARTESIAN_POINT ( 'NONE',  ( 26.38776508739448801, 137.6838126476015134, 8.633687169601740763 ) ) ;
#9901 = VECTOR ( 'NONE', #12540, 1000.000000000000000 ) ;
#9902 = DIRECTION ( 'NONE',  ( 0.000000000000000000, 1.000000000000000000, 0.000000000000000000 ) ) ;
#9903 = FACE_OUTER_BOUND ( 'NONE', #15596, .T. ) ;
#9904 = DIRECTION ( 'NONE',  ( 0.000000000000000000, 0.000000000000000000, 1.000000000000000000 ) ) ;
#9905 = LINE ( 'NONE', #15390, #5293 ) ;
#9906 = DIRECTION ( 'NONE',  ( 0.000000000000000000, 0.000000000000000000, -1.000000000000000000 ) ) ;
#9907 = ADVANCED_FACE ( 'NONE', ( #12220 ), #8142, .F. ) ;
#9908 = EDGE_CURVE ( 'NONE', #6775, #11482, #91, .T. ) ;
#9909 = DIRECTION ( 'NONE',  ( -1.000000000000000000, -0.000000000000000000, -0.000000000000000000 ) ) ;
#9910 = EDGE_CURVE ( 'NONE', #10212, #15075, #7327, .T. ) ;
#9911 = VERTEX_POINT ( 'NONE', #530 ) ;
#9912 = AXIS2_PLACEMENT_3D ( 'NONE', #582, #7211, #13682 ) ;
#9913 = EDGE_LOOP ( 'NONE', ( #15725, #2072 ) ) ;
#9914 = CARTESIAN_POINT ( 'NONE',  ( 24.93507336697333798, 29.86842105264641845, -5.660862367392566874 ) ) ;
#9915 = CIRCLE ( 'NONE', #2282, 10.00000000000000178 ) ;
#9916 = CARTESIAN_POINT ( 'NONE',  ( 24.75325409605274274, 140.3706687641101212, -10.61653890585399296 ) ) ;
#9917 = ORIENTED_EDGE ( 'NONE', *, *, #373, .F. ) ;
#9918 = DIRECTION ( 'NONE',  ( -0.000000000000000000, -0.000000000000000000, -1.000000000000000000 ) ) ;
#9919 = CARTESIAN_POINT ( 'NONE',  ( 49.99999999999998579, 171.6227766016838245, -15.00000337241049131 ) ) ;
#9920 = EDGE_LOOP ( 'NONE', ( #8805, #16615 ) ) ;
#9921 = CARTESIAN_POINT ( 'NONE',  ( 22.65335638526122963, 148.1846496461902234, -23.23759988234781204 ) ) ;
#9922 = VECTOR ( 'NONE', #10023, 1000.000000000000000 ) ;
#9923 = DIRECTION ( 'NONE',  ( -1.000000000000000000, 0.000000000000000000, 0.000000000000000000 ) ) ;
#9924 = DIRECTION ( 'NONE',  ( 1.000000000000000000, -0.000000000000000000, -0.000000000000000000 ) ) ;
#9925 = DIRECTION ( 'NONE',  ( 1.224646799147353207E-16, 1.000000000000000000, 0.000000000000000000 ) ) ;
#9926 = CARTESIAN_POINT ( 'NONE',  ( -48.00000000000000000, 154.3022685259950038, 9.999999999999900524 ) ) ;
#9927 = EDGE_CURVE ( 'NONE', #14513, #4275, #6991, .T. ) ;
#9928 = EDGE_CURVE ( 'NONE', #5121, #3610, #4778, .T. ) ;
#9929 = CARTESIAN_POINT ( 'NONE',  ( -33.00000000000000711, 171.6227766016838245, 5.000000000000007994 ) ) ;
#9930 = LINE ( 'NONE', #15060, #709 ) ;
#9931 = EDGE_LOOP ( 'NONE', ( #10239, #5582, #13958, #8978 ) ) ;
#9932 = CYLINDRICAL_SURFACE ( 'NONE', #9848, 33.00000000000000000 ) ;
#9933 = ORIENTED_EDGE ( 'NONE', *, *, #14528, .F. ) ;
#9934 = CARTESIAN_POINT ( 'NONE',  ( 1.559999999999998943, -0.8660254037844428154, -1.499999999999997780 ) ) ;
#9935 = AXIS2_PLACEMENT_3D ( 'NONE', #13842, #5957, #9745 ) ;
#9936 = CARTESIAN_POINT ( 'NONE',  ( -80.00000000000001421, 196.6227766016838245, -16.00000000000000000 ) ) ;
#9937 = ORIENTED_EDGE ( 'NONE', *, *, #6807, .T. ) ;
#9938 = CARTESIAN_POINT ( 'NONE',  ( -48.00000000000000000, 191.6227766016837961, 1.224646799147353454E-15 ) ) ;
#9939 =( BOUNDED_SURFACE ( )  B_SPLINE_SURFACE ( 3, 2, ( 
 ( #17046, #14396, #6250 ),
 ( #7658, #934, #7735 ),
 ( #6323, #11718, #7570 ),
 ( #14479, #13146, #4842 ),
 ( #10230, #17128, #5005 ),
 ( #10570, #10392, #5179 ),
 ( #14561, #15628, #8893 ),
 ( #15894, #1015, #6419 ),
 ( #11811, #17217, #5095 ),
 ( #3764, #9154, #1848 ),
 ( #12981, #2432, #7830 ),
 ( #15978, #13241, #1112 ),
 ( #6512, #3505, #11905 ),
 ( #17311, #3861, #13986 ),
 ( #12652, #9682, #478 ),
 ( #4383, #5882, #4563 ),
 ( #13947, #16440, #1730 ),
 ( #9948, #5626, #1808 ),
 ( #11019, #16514, #9860 ),
 ( #7203, #5714, #1900 ),
 ( #15348, #7294, #387 ),
 ( #11279, #11186, #9771 ),
 ( #15175, #578, #5977 ),
 ( #4300, #3143, #5789 ),
 ( #8715, #12608, #16694 ),
 ( #7041, #15081, #16603 ),
 ( #3046, #8619, #4476 ),
 ( #14123, #12524, #15268 ) ),
 .UNSPECIFIED., .F., .F., .T. ) 
 B_SPLINE_SURFACE_WITH_KNOTS ( ( 4, 2, 2, 2, 2, 2, 2, 2, 2, 2, 2, 2, 2, 4 ),
 ( 3, 3 ),
 ( 0.01342997177288655399, 0.01733910390705692070, 0.01929366997414210666, 0.02124823604122728915, 0.02515736817539765760, 0.02711193424248284356, 0.02906650030956802605, 0.03297563244373839797, 0.03493019851082358046, 0.03688476457790876295, 0.03883933064499394544, 0.03981661367853653322, 0.04079389671207912793, 0.04470302884624949985 ),
 ( 0.000000000000000000, 1.000000000000000000 ),
 .UNSPECIFIED. ) 
 GEOMETRIC_REPRESENTATION_ITEM ( )  RATIONAL_B_SPLINE_SURFACE ( (
 ( 1.000000000000000000, 0.7117435966472906994, 1.000000000000000000),
 ( 1.000000000000000000, 0.7117434842622243352, 1.000000000000000000),
 ( 1.000000000000000000, 0.7117144184577041122, 1.000000000000000000),
 ( 1.000000000000000000, 0.7116285301813174424, 1.000000000000000000),
 ( 1.000000000000000000, 0.7115928256594988843, 1.000000000000000000),
 ( 1.000000000000000000, 0.7115068832447583036, 1.000000000000000000),
 ( 1.000000000000000000, 0.7114564033772057261, 1.000000000000000000),
 ( 1.000000000000000000, 0.7112861117249480447, 1.000000000000000000),
 ( 1.000000000000000000, 0.7111469280185451769, 1.000000000000000000),
 ( 1.000000000000000000, 0.7108993804763810154, 1.000000000000000000),
 ( 1.000000000000000000, 0.7108100171490865371, 1.000000000000000000),
 ( 1.000000000000000000, 0.7106191415567553182, 1.000000000000000000),
 ( 1.000000000000000000, 0.7105185320923615988, 1.000000000000000000),
 ( 1.000000000000000000, 0.7102014790723295556, 1.000000000000000000),
 ( 1.000000000000000000, 0.7099699576740480245, 1.000000000000000000),
 ( 1.000000000000000000, 0.7095909300315041968, 1.000000000000000000),
 ( 1.000000000000000000, 0.7094593121158984106, 1.000000000000000000),
 ( 1.000000000000000000, 0.7091910831477740151, 1.000000000000000000),
 ( 1.000000000000000000, 0.7090537746377550965, 1.000000000000000000),
 ( 1.000000000000000000, 0.7087727591781153302, 1.000000000000000000),
 ( 1.000000000000000000, 0.7086290523620303317, 1.000000000000000000),
 ( 1.000000000000000000, 0.7084085592173990920, 1.000000000000000000),
 ( 1.000000000000000000, 0.7083342380281847372, 1.000000000000000000),
 ( 1.000000000000000000, 0.7081839094109132482, 1.000000000000000000),
 ( 1.000000000000000000, 0.7081077478408333015, 1.000000000000000000),
 ( 1.000000000000000000, 0.7077267031860466906, 1.000000000000000000),
 ( 1.000000000000000000, 0.7074184602291956336, 1.000000000000000000),
 ( 1.000000000000000000, 0.7071067811865476838, 1.000000000000000000) ) ) 
 REPRESENTATION_ITEM ( '' )  SURFACE ( )  );
#9940 = DIRECTION ( 'NONE',  ( 0.000000000000000000, 0.000000000000000000, 1.000000000000000000 ) ) ;
#9941 = CARTESIAN_POINT ( 'NONE',  ( 16.35719767791491819, 136.8501131444031387, 5.449348266248943418 ) ) ;
#9942 = EDGE_LOOP ( 'NONE', ( #4916, #1105, #3674, #15794 ) ) ;
#9943 = DIRECTION ( 'NONE',  ( 0.000000000000000000, 0.000000000000000000, 1.000000000000000000 ) ) ;
#9944 = EDGE_CURVE ( 'NONE', #6282, #10721, #15219, .T. ) ;
#9945 = DIRECTION ( 'NONE',  ( -0.000000000000000000, -0.000000000000000000, 1.000000000000000000 ) ) ;
#9946 = LINE ( 'NONE', #11535, #14673 ) ;
#9947 = FACE_OUTER_BOUND ( 'NONE', #8365, .T. ) ;
#9948 = CARTESIAN_POINT ( 'NONE',  ( 23.77503517897901375, 18.00000000000000000, 22.95135521423614833 ) ) ;
#9949 = CARTESIAN_POINT ( 'NONE',  ( -7.970809231268917827, 17.99999999998357936, -12.80353734461080428 ) ) ;
#9950 = ORIENTED_EDGE ( 'NONE', *, *, #8573, .T. ) ;
#9951 = CARTESIAN_POINT ( 'NONE',  ( 24.00000000000000000, 196.6227766016838245, -35.00000000000000000 ) ) ;
#9952 = FACE_OUTER_BOUND ( 'NONE', #4903, .T. ) ;
#9953 = ORIENTED_EDGE ( 'NONE', *, *, #13254, .T. ) ;
#9954 = DIRECTION ( 'NONE',  ( 0.000000000000000000, 0.000000000000000000, 1.000000000000000000 ) ) ;
#9955 = DIRECTION ( 'NONE',  ( -1.000000000000000000, -0.000000000000000000, -0.000000000000000000 ) ) ;
#9956 = ORIENTED_EDGE ( 'NONE', *, *, #10082, .F. ) ;
#9957 = VERTEX_POINT ( 'NONE', #11233 ) ;
#9958 = CARTESIAN_POINT ( 'NONE',  ( 9.276452510677492214, 132.6951329324795381, 12.46699917133672741 ) ) ;
#9959 = VERTEX_POINT ( 'NONE', #4258 ) ;
#9960 = VERTEX_POINT ( 'NONE', #350 ) ;
#9961 = FACE_BOUND ( 'NONE', #13879, .T. ) ;
#9962 = ADVANCED_FACE ( 'NONE', ( #13909 ), #8577, .F. ) ;
#9963 = CARTESIAN_POINT ( 'NONE',  ( 196.0000000000000000, 183.6227766016837961, 5.571800142134975431 ) ) ;
#9964 = CARTESIAN_POINT ( 'NONE',  ( 49.99999999999998579, 191.6227766016837677, -5.571800142134975431 ) ) ;
#9965 = CARTESIAN_POINT ( 'NONE',  ( 37.43654228017073393, 145.5167101299681178, -20.20458554073936241 ) ) ;
#9966 = ORIENTED_EDGE ( 'NONE', *, *, #1988, .F. ) ;
#9967 = CARTESIAN_POINT ( 'NONE',  ( 34.48889888759456568, 144.3473407286824965, 18.59810793231920201 ) ) ;
#9968 = DIRECTION ( 'NONE',  ( 0.000000000000000000, -0.8660254037844413721, 0.4999999999999953371 ) ) ;
#9969 = CARTESIAN_POINT ( 'NONE',  ( -100.0000000000000000, 143.0439382767972347, 16.49999999999984368 ) ) ;
#9970 = ADVANCED_FACE ( 'NONE', ( #4338 ), #16474, .F. ) ;
#9971 = CARTESIAN_POINT ( 'NONE',  ( -12.14981508666162036, 19.99999999999315037, -12.53017279448777366 ) ) ;
#9972 = CARTESIAN_POINT ( 'NONE',  ( -48.00000000000000000, 154.3022685259950038, -9.999999999999900524 ) ) ;
#9973 = EDGE_CURVE ( 'NONE', #11927, #2395, #15145, .T. ) ;
#9974 = DIRECTION ( 'NONE',  ( 1.000000000000000000, -0.000000000000000000, -0.000000000000000000 ) ) ;
#9975 = ORIENTED_EDGE ( 'NONE', *, *, #9737, .T. ) ;
#9976 = DIRECTION ( 'NONE',  ( -1.000000000000000000, 0.000000000000000000, 0.000000000000000000 ) ) ;
#9977 = ORIENTED_EDGE ( 'NONE', *, *, #112, .T. ) ;
#9978 = DIRECTION ( 'NONE',  ( 0.01578383822436034076, -0.1110972697184772484, -0.9936841888205766304 ) ) ;
#9979 = VERTEX_POINT ( 'NONE', #3004 ) ;
#9980 = CARTESIAN_POINT ( 'NONE',  ( -195.2299705378136991, 174.0696332146309260, 3.384031243670088784 ) ) ;
#9981 = CARTESIAN_POINT ( 'NONE',  ( -98.00000000000000000, 171.6227766016838245, 0.000000000000000000 ) ) ;
#9982 = ORIENTED_EDGE ( 'NONE', *, *, #1384, .T. ) ;
#9983 = DIRECTION ( 'NONE',  ( -0.000000000000000000, -0.000000000000000000, -1.000000000000000000 ) ) ;
#9984 = DIRECTION ( 'NONE',  ( 0.000000000000000000, 0.000000000000000000, -1.000000000000000000 ) ) ;
#9985 = DIRECTION ( 'NONE',  ( -0.000000000000000000, -0.000000000000000000, 1.000000000000000000 ) ) ;
#9986 = DIRECTION ( 'NONE',  ( 0.000000000000000000, -0.8660254037844388186, -0.4999999999999998335 ) ) ;
#9987 = VERTEX_POINT ( 'NONE', #5750 ) ;
#9988 = VERTEX_POINT ( 'NONE', #1688 ) ;
#9989 = CARTESIAN_POINT ( 'NONE',  ( 24.80291332262510196, 19.99999999999999645, -7.298429162487363620 ) ) ;
#9990 = CARTESIAN_POINT ( 'NONE',  ( -27.98221281347037959, 30.00000000000000000, 0.000000000000000000 ) ) ;
#9991 = ORIENTED_EDGE ( 'NONE', *, *, #12630, .F. ) ;
#9992 = CYLINDRICAL_SURFACE ( 'NONE', #12315, 10.00000000000000000 ) ;
#9993 = DIRECTION ( 'NONE',  ( 0.000000000000000000, 0.000000000000000000, -1.000000000000000000 ) ) ;
#9994 = ORIENTED_EDGE ( 'NONE', *, *, #9881, .F. ) ;
#9995 = EDGE_CURVE ( 'NONE', #6282, #6096, #798, .T. ) ;
#9996 = CARTESIAN_POINT ( 'NONE',  ( 35.59761955342209916, 201.6350306476045091, -13.74486639216963901 ) ) ;
#9997 = DIRECTION ( 'NONE',  ( -0.000000000000000000, -0.000000000000000000, -1.000000000000000000 ) ) ;
#9998 = LINE ( 'NONE', #3200, #12619 ) ;
#9999 = VECTOR ( 'NONE', #16472, 1000.000000000000000 ) ;
#10000 = CARTESIAN_POINT ( 'NONE',  ( -40.00000000000000000, 20.00000000000000000, -30.00000000000000355 ) ) ;
#10001 = CARTESIAN_POINT ( 'NONE',  ( -8.720613081040614389, 18.00000000000000000, 24.99999999951824492 ) ) ;
#10002 = AXIS2_PLACEMENT_3D ( 'NONE', #9217, #16225, #7797 ) ;
#10003 = DIRECTION ( 'NONE',  ( -1.000000000000000000, -0.000000000000000000, -0.000000000000000000 ) ) ;
#10004 = CARTESIAN_POINT ( 'NONE',  ( -72.95161576004603887, 144.0140295085316779, -18.09598853029520171 ) ) ;
#10005 = ORIENTED_EDGE ( 'NONE', *, *, #8412, .F. ) ;
#10006 = CARTESIAN_POINT ( 'NONE',  ( -154.9692839938123257, 171.6227766016838245, 23.61711149033413903 ) ) ;
#10007 = VERTEX_POINT ( 'NONE', #12485 ) ;
#10008 = CARTESIAN_POINT ( 'NONE',  ( -72.50000000000000000, 196.6227766016838245, -21.54065922853802562 ) ) ;
#10009 = CARTESIAN_POINT ( 'NONE',  ( -25.15885279626527549, 18.00000000000000355, -15.13659797665870066 ) ) ;
#10010 = VERTEX_POINT ( 'NONE', #14959 ) ;
#10011 = DIRECTION ( 'NONE',  ( 0.000000000000000000, 0.000000000000000000, 1.000000000000000000 ) ) ;
#10012 = EDGE_CURVE ( 'NONE', #14627, #4871, #3096, .T. ) ;
#10013 = EDGE_CURVE ( 'NONE', #10145, #12789, #7253, .T. ) ;
#10014 = AXIS2_PLACEMENT_3D ( 'NONE', #15332, #7370, #6038 ) ;
#10015 = CARTESIAN_POINT ( 'NONE',  ( 22.87244304995705235, 29.89498257257996272, 11.09085247437311494 ) ) ;
#10016 = EDGE_CURVE ( 'NONE', #13808, #9656, #16935, .T. ) ;
#10017 = CARTESIAN_POINT ( 'NONE',  ( 20.41303537792882139, 140.1262507166239573, 15.26811025958205015 ) ) ;
#10018 = EDGE_LOOP ( 'NONE', ( #16525, #999, #4479, #8552 ) ) ;
#10019 = CONTEXT_DEPENDENT_SHAPE_REPRESENTATION ( #12651, #2067 ) ;
#10020 = CARTESIAN_POINT ( 'NONE',  ( -24.93725393319379435, 120.0000000000000284, 5.500000000000000000 ) ) ;
#10021 = CYLINDRICAL_SURFACE ( 'NONE', #3281, 2.499999999999998668 ) ;
#10022 = CARTESIAN_POINT ( 'NONE',  ( -76.34901055807858938, 193.2024116766813506, 24.96685975555418224 ) ) ;
#10023 = DIRECTION ( 'NONE',  ( -0.000000000000000000, 1.000000000000000000, 0.000000000000000000 ) ) ;
#10024 =( REPRESENTATION_RELATIONSHIP ('NONE','NONE', #9723, #17073 ) REPRESENTATION_RELATIONSHIP_WITH_TRANSFORMATION ( #16508 )SHAPE_REPRESENTATION_RELATIONSHIP( ) );
#10025 = CARTESIAN_POINT ( 'NONE',  ( 196.0000000000000000, 163.6227766016838530, 12.50000337241049309 ) ) ;
#10026 = CARTESIAN_POINT ( 'NONE',  ( -197.9999999999999716, 189.6227766016838245, 0.000000000000000000 ) ) ;
#10027 = AXIS2_PLACEMENT_3D ( 'NONE', #4101, #14977, #10737 ) ;
#10028 = ORIENTED_EDGE ( 'NONE', *, *, #994, .F. ) ;
#10029 = LINE ( 'NONE', #581, #3050 ) ;
#10031 = CARTESIAN_POINT ( 'NONE',  ( -27.98221281347037959, 20.00000000000000355, -5.670874406215274277 ) ) ;
#10030 = VECTOR ( 'NONE', #2564, 1000.000000000000000 ) ;
#10032 = EDGE_LOOP ( 'NONE', ( #5518, #17104, #8729 ) ) ;
#10033 = CARTESIAN_POINT ( 'NONE',  ( -96.00000000000001421, 171.6227766016838245, -30.00000000000000000 ) ) ;
#10034 = CIRCLE ( 'NONE', #8906, 10.00000000000000178 ) ;
#10035 = CARTESIAN_POINT ( 'NONE',  ( -151.0000000000000284, 196.6227766016838245, 0.000000000000000000 ) ) ;
#10036 = ORIENTED_EDGE ( 'NONE', *, *, #13706, .T. ) ;
#10037 = VERTEX_POINT ( 'NONE', #4688 ) ;
#10038 = ORIENTED_EDGE ( 'NONE', *, *, #2843, .T. ) ;
#10039 = CARTESIAN_POINT ( 'NONE',  ( 48.00000000000000711, 175.6227766016838530, 21.92820660268601074 ) ) ;
#10040 = ORIENTED_EDGE ( 'NONE', *, *, #12951, .T. ) ;
#10041 = DIRECTION ( 'NONE',  ( -0.000000000000000000, -0.000000000000000000, -1.000000000000000000 ) ) ;
#10042 = VECTOR ( 'NONE', #3425, 1000.000000000000000 ) ;
#10043 = ORIENTED_EDGE ( 'NONE', *, *, #14669, .F. ) ;
#10044 = CARTESIAN_POINT ( 'NONE',  ( 24.10786375645522384, 141.9593924407984957, -14.48320912595415244 ) ) ;
#10045 = AXIS2_PLACEMENT_3D ( 'NONE', #14404, #6082, #12988 ) ;
#10046 = VECTOR ( 'NONE', #4552, 1000.000000000000000 ) ;
#10047 = PRESENTATION_STYLE_ASSIGNMENT (( #2009 ) ) ;
#10048 = CARTESIAN_POINT ( 'NONE',  ( -27.98221281347037959, 30.00000000000000000, 0.000000000000000000 ) ) ;
#10049 = CARTESIAN_POINT ( 'NONE',  ( 48.00000000000000711, 159.6227766016838814, -8.071800142134975431 ) ) ;
#10050 = ORIENTED_EDGE ( 'NONE', *, *, #12478, .F. ) ;
#10051 = CARTESIAN_POINT ( 'NONE',  ( -45.00000000000000711, 171.6227766016838245, 0.000000000000000000 ) ) ;
#10052 = CARTESIAN_POINT ( 'NONE',  ( -44.99999999999997158, 8.000000000000000000, -40.00000000000000000 ) ) ;
#10053 = DIRECTION ( 'NONE',  ( -0.000000000000000000, -0.000000000000000000, 1.000000000000000000 ) ) ;
#10054 = CARTESIAN_POINT ( 'NONE',  ( -14.55266450408011636, 19.99999999999999645, -23.76398220081675206 ) ) ;
#10055 = CARTESIAN_POINT ( 'NONE',  ( -50.00000000000000000, 8.000000000000000000, -35.00000000000000000 ) ) ;
#10056 = AXIS2_PLACEMENT_3D ( 'NONE', #207, #11002, #7449 ) ;
#10057 = CIRCLE ( 'NONE', #14030, 2.500000000000002220 ) ;
#10058 = AXIS2_PLACEMENT_3D ( 'NONE', #15727, #947, #7942 ) ;
#10059 = EDGE_CURVE ( 'NONE', #14104, #15177, #6097, .T. ) ;
#10060 = AXIS2_PLACEMENT_3D ( 'NONE', #4485, #397, #15012 ) ;
#10061 = EDGE_CURVE ( 'NONE', #13439, #12155, #9578, .T. ) ;
#10062 = CARTESIAN_POINT ( 'NONE',  ( -80.00000000000001421, 196.6227766016838245, -16.00000000000000000 ) ) ;
#10063 = VERTEX_POINT ( 'NONE', #10170 ) ;
#10064 = DIRECTION ( 'NONE',  ( 0.000000000000000000, 0.000000000000000000, 1.000000000000000000 ) ) ;
#10065 = EDGE_LOOP ( 'NONE', ( #3983, #5261, #3335, #784 ) ) ;
#10066 =( NAMED_UNIT ( * ) PLANE_ANGLE_UNIT ( ) SI_UNIT ( $, .RADIAN. ) );
#10067 = CARTESIAN_POINT ( 'NONE',  ( -95.00000000000000000, 201.6227766016838245, 0.000000000000000000 ) ) ;
#10068 = EDGE_CURVE ( 'NONE', #9898, #14250, #261, .T. ) ;
#10069 = VECTOR ( 'NONE', #1077, 1000.000000000000000 ) ;
#10070 = AXIS2_PLACEMENT_3D ( 'NONE', #5509, #14890, #6761 ) ;
#10071 = DIRECTION ( 'NONE',  ( 0.000000000000000000, 0.000000000000000000, 1.000000000000000000 ) ) ;
#10072 = VECTOR ( 'NONE', #1333, 1000.000000000000000 ) ;
#10073 = CARTESIAN_POINT ( 'NONE',  ( 0.000000000000000000, 0.000000000000000000, 0.000000000000000000 ) ) ;
#10074 = AXIS2_PLACEMENT_3D ( 'NONE', #14316, #3438, #4596 ) ;
#10075 = EDGE_LOOP ( 'NONE', ( #64, #4342, #16688, #15880 ) ) ;
#10076 = CARTESIAN_POINT ( 'NONE',  ( 20.49999999999998224, 10.00000000000000000, -35.00200000000000244 ) ) ;
#10077 = DIRECTION ( 'NONE',  ( 0.000000000000000000, 0.000000000000000000, 1.000000000000000000 ) ) ;
#10078 = CARTESIAN_POINT ( 'NONE',  ( -84.01788347118190359, 199.6128501304145004, 17.48539201980444346 ) ) ;
#10079 = CARTESIAN_POINT ( 'NONE',  ( 24.04231242562121551, 197.3572491277162158, -23.72357542124676044 ) ) ;
#10080 = ORIENTED_EDGE ( 'NONE', *, *, #12304, .T. ) ;
#10081 = ORIENTED_EDGE ( 'NONE', *, *, #12533, .T. ) ;
#10082 = EDGE_CURVE ( 'NONE', #15131, #16992, #15391, .T. ) ;
#10083 = CARTESIAN_POINT ( 'NONE',  ( 18.47379060770018810, 20.00000000000225953, -14.40819024183099728 ) ) ;
#10084 = B_SPLINE_CURVE_WITH_KNOTS ( 'NONE', 3,
 ( #10469, #17372, #7548, #6302 ),
 .UNSPECIFIED., .F., .F.,
 ( 4, 4 ),
 ( 0.000000000000000000, 0.0004807729677303993116 ),
 .UNSPECIFIED. ) ;
#10085 = DIRECTION ( 'NONE',  ( 0.9961946980917461003, 0.08715574274765185148, 0.000000000000000000 ) ) ;
#10086 = VERTEX_POINT ( 'NONE', #16816 ) ;
#10087 = DIRECTION ( 'NONE',  ( 0.000000000000000000, 0.000000000000000000, 1.000000000000000000 ) ) ;
#10088 = MECHANICAL_DESIGN_GEOMETRIC_PRESENTATION_REPRESENTATION (  '', ( #1620 ), #3887 ) ;
#10089 = CARTESIAN_POINT ( 'NONE',  ( -87.50000000000004263, 146.6227766016838245, -35.00200000000000244 ) ) ;
#10090 = EDGE_CURVE ( 'NONE', #11495, #11331, #9289, .T. ) ;
#10091 = VERTEX_POINT ( 'NONE', #795 ) ;
#10092 = CARTESIAN_POINT ( 'NONE',  ( 34.99999999999999289, -20.00000000000000000, -40.00000000000001421 ) ) ;
#10093 = ADVANCED_FACE ( 'NONE', ( #15483 ), #15650, .F. ) ;
#10094 = EDGE_CURVE ( 'NONE', #2358, #6948, #16385, .T. ) ;
#10095 = CARTESIAN_POINT ( 'NONE',  ( 196.0000000000000000, 155.6227766016839098, -12.50000337241049309 ) ) ;
#10096 = CARTESIAN_POINT ( 'NONE',  ( -40.00000000000000000, 4.000000000000000000, -33.00000000000000711 ) ) ;
#10097 = CARTESIAN_POINT ( 'NONE',  ( -12.79675654462651124, 18.00000000000000355, 5.581853174322293221 ) ) ;
#10098 = AXIS2_PLACEMENT_3D ( 'NONE', #1490, #6718, #12277 ) ;
#10099 = LINE ( 'NONE', #15506, #16531 ) ;
#10100 = AXIS2_PLACEMENT_3D ( 'NONE', #6136, #7774, #3723 ) ;
#10101 = DIRECTION ( 'NONE',  ( -1.000000000000000000, 0.000000000000000000, 0.000000000000000000 ) ) ;
#10102 = ORIENTED_EDGE ( 'NONE', *, *, #5092, .F. ) ;
#10103 = CYLINDRICAL_SURFACE ( 'NONE', #7582, 11.99999999999999645 ) ;
#10104 = EDGE_CURVE ( 'NONE', #16267, #11049, #7875, .T. ) ;
#10105 = ORIENTED_EDGE ( 'NONE', *, *, #5108, .T. ) ;
#10106 = CARTESIAN_POINT ( 'NONE',  ( -45.00000000000000000, 120.0000000000000142, -15.00000000000000000 ) ) ;
#10107 = CARTESIAN_POINT ( 'NONE',  ( -27.81025873171734375, 18.00000000000000355, -7.666431193274476641 ) ) ;
#10108 = ORIENTED_EDGE ( 'NONE', *, *, #6850, .T. ) ;
#10109 = CARTESIAN_POINT ( 'NONE',  ( 30.00000000000001066, 146.6227766016838245, 0.000000000000000000 ) ) ;
#10110 = CARTESIAN_POINT ( 'NONE',  ( 23.71167364621568652, 19.99999999999772982, 10.06760101871518032 ) ) ;
#10111 = CARTESIAN_POINT ( 'NONE',  ( 34.99999999999999289, 8.000000000000010658, 40.00000000000000711 ) ) ;
#10112 = STYLED_ITEM ( 'NONE', ( #9696 ), #8036 ) ;
#10113 = ORIENTED_EDGE ( 'NONE', *, *, #4947, .T. ) ;
#10114 = CYLINDRICAL_SURFACE ( 'NONE', #4131, 27.69059892324149530 ) ;
#10115 = B_SPLINE_CURVE_WITH_KNOTS ( 'NONE', 3,
 ( #1262, #12062, #17471, #16151, #4023, #638, #7101, #448, #4624, #5857, #11513, #1962, #8691, #367 ),
 .UNSPECIFIED., .F., .F.,
 ( 4, 2, 2, 2, 2, 2, 4 ),
 ( 0.000000000000000000, 0.0006954478661159615820, 0.001043171799173978802, 0.001390895732231996239, 0.001738619665290013242, 0.002086343598348030463, 0.002781791464464176359 ),
 .UNSPECIFIED. ) ;
#10116 = DIRECTION ( 'NONE',  ( -1.000000000000000000, -0.000000000000000000, 0.000000000000000000 ) ) ;
#10117 = CARTESIAN_POINT ( 'NONE',  ( -17.63576980228536328, 32.18555361985414720, -8.400096275226864861 ) ) ;
#10118 = DIRECTION ( 'NONE',  ( 0.000000000000000000, -0.5000000000000011102, -0.8660254037844379305 ) ) ;
#10119 = PRODUCT_DEFINITION_SHAPE ( 'NONE', 'NONE',  #17534 ) ;
#10120 = CARTESIAN_POINT ( 'NONE',  ( -91.33974596215561803, 206.6227766016838245, 0.000000000000000000 ) ) ;
#10121 = ORIENTED_EDGE ( 'NONE', *, *, #6112, .T. ) ;
#10122 = CARTESIAN_POINT ( 'NONE',  ( 15.00000000000000000, 171.6227766016838245, 0.000000000000000000 ) ) ;
#10123 = ADVANCED_FACE ( 'NONE', ( #7597 ), #8671, .T. ) ;
#10124 = ADVANCED_FACE ( 'NONE', ( #3527 ), #16904, .T. ) ;
#10125 = VECTOR ( 'NONE', #14711, 1000.000000000000000 ) ;
#10126 = CARTESIAN_POINT ( 'NONE',  ( 2.370000000000000551, 4.750000000000000888, 0.000000000000000000 ) ) ;
#10127 = ADVANCED_FACE ( 'NONE', ( #3450 ), #4503, .T. ) ;
#10128 = ORIENTED_EDGE ( 'NONE', *, *, #995, .T. ) ;
#10129 = DIRECTION ( 'NONE',  ( 0.000000000000000000, 0.000000000000000000, -1.000000000000000000 ) ) ;
#10130 = CIRCLE ( 'NONE', #10988, 33.00000000000000000 ) ;
#10131 = FACE_BOUND ( 'NONE', #860, .T. ) ;
#10132 = ADVANCED_FACE ( 'NONE', ( #1942 ), #619, .F. ) ;
#10133 = ORIENTED_EDGE ( 'NONE', *, *, #15927, .F. ) ;
#10134 = ORIENTED_EDGE ( 'NONE', *, *, #9371, .F. ) ;
#10135 = ORIENTED_EDGE ( 'NONE', *, *, #1278, .F. ) ;
#10136 = CARTESIAN_POINT ( 'NONE',  ( -68.00000000000000000, 171.6227766016838245, -19.49999999999998934 ) ) ;
#10137 = AXIS2_PLACEMENT_3D ( 'NONE', #8759, #704, #10330 ) ;
#10138 = VERTEX_POINT ( 'NONE', #15741 ) ;
#10139 = SURFACE_STYLE_FILL_AREA ( #8640 ) ;
#10140 =( REPRESENTATION_RELATIONSHIP ('NONE','NONE', #9723, #7924 ) REPRESENTATION_RELATIONSHIP_WITH_TRANSFORMATION ( #15432 )SHAPE_REPRESENTATION_RELATIONSHIP( ) );
#10141 = CARTESIAN_POINT ( 'NONE',  ( -40.00000000000000000, 4.000000000000000000, -33.00000000000000711 ) ) ;
#10142 = CARTESIAN_POINT ( 'NONE',  ( 7.743794661876905572, 133.6328069455646528, 12.86244959688548128 ) ) ;
#10143 = DIRECTION ( 'NONE',  ( -0.000000000000000000, -0.000000000000000000, 1.000000000000000000 ) ) ;
#10144 = LINE ( 'NONE', #2345, #17399 ) ;
#10145 = VERTEX_POINT ( 'NONE', #9009 ) ;
#10146 = CARTESIAN_POINT ( 'NONE',  ( 30.46461711770098546, 141.6391889668067563, 13.78368973859836011 ) ) ;
#10147 = CARTESIAN_POINT ( 'NONE',  ( -80.00000000000001421, 196.6227766016838245, 10.00000000000000178 ) ) ;
#10148 = ADVANCED_FACE ( 'NONE', ( #14082 ), #2288, .F. ) ;
#10149 = CARTESIAN_POINT ( 'NONE',  ( -75.00000000000002842, 146.6227766016838245, 35.00200000000000244 ) ) ;
#10150 = CARTESIAN_POINT ( 'NONE',  ( -22.80699178664306004, 19.99999999999999645, -18.33022619056923119 ) ) ;
#10151 = EDGE_CURVE ( 'NONE', #1517, #6848, #16091, .T. ) ;
#10152 = DIRECTION ( 'NONE',  ( 1.000000000000000000, -1.243449787580175325E-14, 0.000000000000000000 ) ) ;
#10153 = CIRCLE ( 'NONE', #4792, 9.999999999999998224 ) ;
#10154 = CIRCLE ( 'NONE', #17230, 19.49999999999998934 ) ;
#10155 = CIRCLE ( 'NONE', #3954, 2.500000000000002220 ) ;
#10156 = CARTESIAN_POINT ( 'NONE',  ( 0.000000000000000000, 20.00000000000000000, 0.000000000000000000 ) ) ;
#10157 = ORIENTED_EDGE ( 'NONE', *, *, #2718, .T. ) ;
#10158 = CARTESIAN_POINT ( 'NONE',  ( -85.27494917608791525, 141.2912748254776147, -13.00000000000000000 ) ) ;
#10159 = ORIENTED_EDGE ( 'NONE', *, *, #17062, .T. ) ;
#10160 =( NAMED_UNIT ( * ) SI_UNIT ( $, .STERADIAN. ) SOLID_ANGLE_UNIT ( ) );
#10161 = CARTESIAN_POINT ( 'NONE',  ( -85.86147415632849800, 195.3295718346067531, -25.74952675241122080 ) ) ;
#10162 = VECTOR ( 'NONE', #11671, 1000.000000000000000 ) ;
#10163 = CARTESIAN_POINT ( 'NONE',  ( 49.99999999999998579, 175.6227766016838245, -3.071800142134975431 ) ) ;
#10164 = AXIS2_PLACEMENT_3D ( 'NONE', #3510, #12897, #15716 ) ;
#10165 = EDGE_CURVE ( 'NONE', #10977, #7447, #10514, .T. ) ;
#10166 = AXIS2_PLACEMENT_3D ( 'NONE', #13573, #5158, #1354 ) ;
#10167 = CARTESIAN_POINT ( 'NONE',  ( -151.9615242270660929, 171.6227766016838245, 0.000000000000000000 ) ) ;
#10168 = ORIENTED_EDGE ( 'NONE', *, *, #4203, .T. ) ;
#10169 = DIRECTION ( 'NONE',  ( 0.000000000000000000, 0.000000000000000000, 1.000000000000000000 ) ) ;
#10170 = CARTESIAN_POINT ( 'NONE',  ( 2.749999999999999112, 5.817072295949927426E-16, -4.750000000000000000 ) ) ;
#10171 = CARTESIAN_POINT ( 'NONE',  ( -75.00000000000000000, 196.6227766016838245, -12.99999999999999822 ) ) ;
#10172 = CARTESIAN_POINT ( 'NONE',  ( 30.28723734794761313, 202.6220268295897426, -16.24950730846250835 ) ) ;
#10173 = VERTEX_POINT ( 'NONE', #6719 ) ;
#10174 = EDGE_LOOP ( 'NONE', ( #9842, #126, #119, #10975 ) ) ;
#10175 = CARTESIAN_POINT ( 'NONE',  ( 23.18512258076559007, 19.99999999999999645, -23.22991426836919260 ) ) ;
#10176 = VECTOR ( 'NONE', #8107, 1000.000000000000000 ) ;
#10177 = VECTOR ( 'NONE', #9909, 1000.000000000000000 ) ;
#10178 = LINE ( 'NONE', #11338, #15163 ) ;
#10179 = EDGE_LOOP ( 'NONE', ( #14535, #6332, #12430, #11238 ) ) ;
#10180 = CYLINDRICAL_SURFACE ( 'NONE', #1608, 19.49999999999998934 ) ;
#10181 = AXIS2_PLACEMENT_3D ( 'NONE', #14933, #13525, #13885 ) ;
#10182 = DIRECTION ( 'NONE',  ( -1.000000000000000000, -0.000000000000000000, -0.000000000000000000 ) ) ;
#10183 = EDGE_LOOP ( 'NONE', ( #2598, #2422 ) ) ;
#10184 = DIRECTION ( 'NONE',  ( -0.08715574274764653628, -0.4980973490458781017, 0.8627299156628190913 ) ) ;
#10185 = UNCERTAINTY_MEASURE_WITH_UNIT (LENGTH_MEASURE( 1.000000000000000082E-05 ), #8373, 'distance_accuracy_value', 'NONE');
#10186 = EDGE_CURVE ( 'NONE', #11799, #3129, #4064, .T. ) ;
#10187 = DIRECTION ( 'NONE',  ( 0.000000000000000000, 0.000000000000000000, 1.000000000000000000 ) ) ;
#10188 = DIRECTION ( 'NONE',  ( 0.000000000000000000, 0.000000000000000000, 1.000000000000000000 ) ) ;
#10189 = AXIS2_PLACEMENT_3D ( 'NONE', #1475, #3962, #14754 ) ;
#10190 = CARTESIAN_POINT ( 'NONE',  ( -15.37626115774789248, 32.49812920269235406, 8.581855491731886332 ) ) ;
#10191 = CARTESIAN_POINT ( 'NONE',  ( -32.65377812985507688, 119.1901795341116923, 4.906772862994290385 ) ) ;
#10192 = AXIS2_PLACEMENT_3D ( 'NONE', #404, #7224, #12625 ) ;
#10193 = DIRECTION ( 'NONE',  ( -1.156482317317868274E-16, 1.000000000000000000, 0.000000000000000000 ) ) ;
#10194 = ORIENTED_EDGE ( 'NONE', *, *, #4895, .F. ) ;
#10195 = CARTESIAN_POINT ( 'NONE',  ( 22.50000000000001421, 146.6227766016838245, -13.00000000000000000 ) ) ;
#10196 = PRODUCT_RELATED_PRODUCT_CATEGORY ( 'part', '', ( #3197 ) ) ;
#10197 = VERTEX_POINT ( 'NONE', #11839 ) ;
#10198 = EDGE_CURVE ( 'NONE', #12616, #13477, #13251, .T. ) ;
#10199 = CARTESIAN_POINT ( 'NONE',  ( -82.50000000000002842, 146.6227766016838245, 10.00000000000000178 ) ) ;
#10200 = EDGE_CURVE ( 'NONE', #12465, #4289, #5359, .T. ) ;
#10201 = CARTESIAN_POINT ( 'NONE',  ( -153.0000000000000284, 171.6227766016838245, 21.61734737250326077 ) ) ;
#10202 = ORIENTED_EDGE ( 'NONE', *, *, #10666, .F. ) ;
#10203 = CARTESIAN_POINT ( 'NONE',  ( 34.80468147095351128, 20.00000000000000000, 7.619145204522578041 ) ) ;
#10204 = CIRCLE ( 'NONE', #10765, 19.49999999999999645 ) ;
#10205 = CARTESIAN_POINT ( 'NONE',  ( 24.29786737972285238, 29.87659578631513568, 8.527395788633878482 ) ) ;
#10206 = ORIENTED_EDGE ( 'NONE', *, *, #1656, .T. ) ;
#10207 = DIRECTION ( 'NONE',  ( 0.000000000000000000, -0.000000000000000000, -1.000000000000000000 ) ) ;
#10208 = CARTESIAN_POINT ( 'NONE',  ( -75.01973743086520585, 196.1036955441148280, 22.13227804827260314 ) ) ;
#10209 = CARTESIAN_POINT ( 'NONE',  ( -14.60673078645093703, 31.57037919282903360, -12.49506642855920724 ) ) ;
#10210 = DIRECTION ( 'NONE',  ( -0.000000000000000000, -0.000000000000000000, -1.000000000000000000 ) ) ;
#10211 = FACE_BOUND ( 'NONE', #14710, .T. ) ;
#10212 = VERTEX_POINT ( 'NONE', #2731 ) ;
#10213 = CYLINDRICAL_SURFACE ( 'NONE', #10688, 750.0000000000001137 ) ;
#10214 = VECTOR ( 'NONE', #8072, 1000.000000000000000 ) ;
#10215 = CARTESIAN_POINT ( 'NONE',  ( -7.379000772444994638, 20.00000000000000000, -25.00000000000000000 ) ) ;
#10216 = EDGE_LOOP ( 'NONE', ( #12506, #4962 ) ) ;
#10217 = CARTESIAN_POINT ( 'NONE',  ( 28.87291500020774393, 190.7253031951458411, -29.32741221247050234 ) ) ;
#10218 = CARTESIAN_POINT ( 'NONE',  ( -95.00000000000000000, 171.6227766016838245, 0.000000000000000000 ) ) ;
#10219 = ORIENTED_EDGE ( 'NONE', *, *, #16103, .F. ) ;
#10220 = ORIENTED_EDGE ( 'NONE', *, *, #8190, .T. ) ;
#10221 = ORIENTED_EDGE ( 'NONE', *, *, #13567, .F. ) ;
#10222 = ORIENTED_EDGE ( 'NONE', *, *, #3444, .T. ) ;
#10223 = CARTESIAN_POINT ( 'NONE',  ( -83.78675088369342916, 153.1023373578139797, -27.31345131271289972 ) ) ;
#10224 = EDGE_LOOP ( 'NONE', ( #14318, #11193, #10635, #13011, #5329, #9488, #3075, #14651, #1099, #13137 ) ) ;
#10225 = PRODUCT_CONTEXT ( 'NONE', #13664, 'mechanical' ) ;
#10226 = EDGE_CURVE ( 'NONE', #11460, #13611, #6628, .T. ) ;
#10227 = DIRECTION ( 'NONE',  ( 0.000000000000000000, 0.000000000000000000, -1.000000000000000000 ) ) ;
#10228 = CARTESIAN_POINT ( 'NONE',  ( -40.00000000000000000, 20.00000000000000000, -30.00000000000000355 ) ) ;
#10229 = FACE_OUTER_BOUND ( 'NONE', #1187, .T. ) ;
#10230 = CARTESIAN_POINT ( 'NONE',  ( 34.26467700469002153, 18.00000000000000000, 10.17319632352554137 ) ) ;
#10231 = DIRECTION ( 'NONE',  ( 0.000000000000000000, 1.000000000000000000, 0.000000000000000000 ) ) ;
#10232 = ORIENTED_EDGE ( 'NONE', *, *, #11046, .F. ) ;
#10233 = CARTESIAN_POINT ( 'NONE',  ( 2.950000000000001066, 3.061616997868382155E-16, -2.499999999999999112 ) ) ;
#10234 = CARTESIAN_POINT ( 'NONE',  ( 49.99999999999998579, 167.6227766016838530, -5.571800142134975431 ) ) ;
#10235 = CARTESIAN_POINT ( 'NONE',  ( -15.00000000000001421, 20.00000000000004263, 4.999999999999999112 ) ) ;
#10236 = CARTESIAN_POINT ( 'NONE',  ( -10.59078875499043981, 19.99999999999999645, -13.69642986623834702 ) ) ;
#10237 = CARTESIAN_POINT ( 'NONE',  ( 2.749999999999999112, 0.000000000000000000, 0.000000000000000000 ) ) ;
#10238 = CARTESIAN_POINT ( 'NONE',  ( 29.39065902011773446, 201.5868197762109730, 13.82597759728686349 ) ) ;
#10239 = ORIENTED_EDGE ( 'NONE', *, *, #3557, .T. ) ;
#10240 = DIRECTION ( 'NONE',  ( -0.000000000000000000, -0.000000000000000000, -1.000000000000000000 ) ) ;
#10241 = ORIENTED_EDGE ( 'NONE', *, *, #8453, .F. ) ;
#10242 = EDGE_CURVE ( 'NONE', #6658, #12961, #2494, .T. ) ;
#10243 = ADVANCED_FACE ( 'NONE', ( #5201, #6542 ), #3710, .T. ) ;
#10244 = CARTESIAN_POINT ( 'NONE',  ( 49.99999999999998579, 167.6227766016838530, -8.071800142134975431 ) ) ;
#10245 = EDGE_CURVE ( 'NONE', #9038, #14903, #13281, .T. ) ;
#10246 = EDGE_CURVE ( 'NONE', #14256, #3772, #14771, .T. ) ;
#10247 = LINE ( 'NONE', #5930, #10411 ) ;
#10248 = CARTESIAN_POINT ( 'NONE',  ( 8.630636718464335999, 133.1548047818457690, -12.68018750699619268 ) ) ;
#10249 = ORIENTED_EDGE ( 'NONE', *, *, #16389, .T. ) ;
#10250 = CARTESIAN_POINT ( 'NONE',  ( 16.17028938446068764, 143.0439382767918346, 16.49999999999050360 ) ) ;
#10251 = DIRECTION ( 'NONE',  ( 1.000000000000000000, 0.000000000000000000, 0.000000000000000000 ) ) ;
#10252 = PLANE ( 'NONE',  #2254 ) ;
#10253 =( NAMED_UNIT ( * ) PLANE_ANGLE_UNIT ( ) SI_UNIT ( $, .RADIAN. ) );
#10254 = EDGE_LOOP ( 'NONE', ( #11378, #8728 ) ) ;
#10255 = ORIENTED_EDGE ( 'NONE', *, *, #8085, .T. ) ;
#10256 = CARTESIAN_POINT ( 'NONE',  ( 17.04141343047935564, 29.97166846511136029, -14.77658840773744409 ) ) ;
#10257 = DIRECTION ( 'NONE',  ( -1.000000000000000000, -0.000000000000000000, 0.000000000000000000 ) ) ;
#10258 = ORIENTED_EDGE ( 'NONE', *, *, #6080, .T. ) ;
#10259 = EDGE_CURVE ( 'NONE', #12789, #2141, #8030, .T. ) ;
#10260 = CARTESIAN_POINT ( 'NONE',  ( -102.0000000000000142, 171.6227766016838245, 25.69059892324149175 ) ) ;
#10261 = DIRECTION ( 'NONE',  ( 1.000000000000000000, 0.000000000000000000, 0.000000000000000000 ) ) ;
#10262 = EDGE_LOOP ( 'NONE', ( #1556, #8461, #3239, #4575, #6717, #16679, #99, #10105 ) ) ;
#10263 = DIRECTION ( 'NONE',  ( 0.000000000000000000, 0.000000000000000000, 1.000000000000000000 ) ) ;
#10264 = PLANE ( 'NONE',  #14321 ) ;
#10265 = CARTESIAN_POINT ( 'NONE',  ( 27.50000000000001066, 146.6227766016838245, 0.000000000000000000 ) ) ;
#10266 = CARTESIAN_POINT ( 'NONE',  ( -24.81085081034726869, 18.00000000000000000, 15.69149817755460496 ) ) ;
#10267 = DIRECTION ( 'NONE',  ( -1.000000000000000000, 0.000000000000000000, 0.000000000000000000 ) ) ;
#10268 = CARTESIAN_POINT ( 'NONE',  ( 35.86376614940371610, 145.1725333695280256, -22.94453145061437382 ) ) ;
#10269 = EDGE_LOOP ( 'NONE', ( #7649, #2026, #8630, #11409 ) ) ;
#10270 = CARTESIAN_POINT ( 'NONE',  ( 4.755015822784812052, 0.000000000000000000, 0.000000000000000000 ) ) ;
#10271 = ORIENTED_EDGE ( 'NONE', *, *, #12254, .T. ) ;
#10272 = CYLINDRICAL_SURFACE ( 'NONE', #12423, 24.99999999999999645 ) ;
#10273 = CARTESIAN_POINT ( 'NONE',  ( -80.00000000000002842, 146.6227766016838245, -35.00200000000000244 ) ) ;
#10274 = ADVANCED_FACE ( 'NONE', ( #17423 ), #2370, .F. ) ;
#10275 = ORIENTED_EDGE ( 'NONE', *, *, #8629, .F. ) ;
#10276 = EDGE_CURVE ( 'NONE', #4551, #13275, #3985, .T. ) ;
#10277 = CARTESIAN_POINT ( 'NONE',  ( 19.49710218362280045, 19.99999999999999289, 24.48336163992366465 ) ) ;
#10278 = CARTESIAN_POINT ( 'NONE',  ( 28.14717441101472772, 19.99999999999999645, 20.07001214883818108 ) ) ;
#10279 = AXIS2_PLACEMENT_3D ( 'NONE', #3524, #6442, #2194 ) ;
#10280 = ORIENTED_EDGE ( 'NONE', *, *, #658, .F. ) ;
#10281 = FACE_OUTER_BOUND ( 'NONE', #1629, .T. ) ;
#10282 = EDGE_CURVE ( 'NONE', #11263, #6590, #6778, .T. ) ;
#10283 = DIRECTION ( 'NONE',  ( -0.000000000000000000, 1.000000000000000000, 0.000000000000000000 ) ) ;
#10284 = CARTESIAN_POINT ( 'NONE',  ( -34.99999999999999289, 130.0000000000000000, 0.000000000000000000 ) ) ;
#10285 = CARTESIAN_POINT ( 'NONE',  ( -21.36854569161881301, 18.00000000000000000, -19.70709815271291632 ) ) ;
#10286 = ORIENTED_EDGE ( 'NONE', *, *, #6451, .T. ) ;
#10287 = CARTESIAN_POINT ( 'NONE',  ( 35.00000000000000000, 196.6227766016838245, 35.00200000000000244 ) ) ;
#10288 = CARTESIAN_POINT ( 'NONE',  ( -14.54670497998687217, 20.00000000000000000, -23.76610458325320607 ) ) ;
#10289 = ORIENTED_EDGE ( 'NONE', *, *, #8575, .F. ) ;
#10290 = CARTESIAN_POINT ( 'NONE',  ( 25.68328880728000030, 192.4368082929522075, -28.14105258436205403 ) ) ;
#10291 = DIRECTION ( 'NONE',  ( 0.000000000000000000, 0.000000000000000000, 1.000000000000000000 ) ) ;
#10292 = EDGE_LOOP ( 'NONE', ( #4597, #1751, #3937, #16066 ) ) ;
#10293 = COLOUR_RGB ( '', 0.40784314, 0.44705882, 0.49803922) ;
#10294 = ORIENTED_EDGE ( 'NONE', *, *, #5991, .F. ) ;
#10295 = ORIENTED_EDGE ( 'NONE', *, *, #1598, .F. ) ;
#10296 = CARTESIAN_POINT ( 'NONE',  ( -72.65282855708331056, 148.1823054118431742, -23.23525722188764675 ) ) ;
#10297 = PRODUCT_DEFINITION ( 'UNKNOWN', '', #3332, #11026 ) ;
#10298 = ORIENTED_EDGE ( 'NONE', *, *, #10666, .T. ) ;
#10299 = DIRECTION ( 'NONE',  ( 1.000000000000000000, 0.000000000000000000, 0.000000000000000000 ) ) ;
#10300 = CARTESIAN_POINT ( 'NONE',  ( -18.23240235453911140, 32.30379688028049401, 5.697301546657946858 ) ) ;
#10301 = ADVANCED_FACE ( 'NONE', ( #15295 ), #1833, .T. ) ;
#10302 = CIRCLE ( 'NONE', #17101, 27.69059892324149530 ) ;
#10303 = CARTESIAN_POINT ( 'NONE',  ( 30.44099542279310810, 152.6108673192418905, -29.38619085311482237 ) ) ;
#10304 = CARTESIAN_POINT ( 'NONE',  ( 196.0000000000000000, 151.6227766016839098, -8.071800142134973655 ) ) ;
#10305 = DIRECTION ( 'NONE',  ( -8.673617379884036705E-17, 0.000000000000000000, 1.000000000000000000 ) ) ;
#10306 = AXIS2_PLACEMENT_3D ( 'NONE', #7019, #4359, #11680 ) ;
#10307 = ORIENTED_EDGE ( 'NONE', *, *, #3391, .T. ) ;
#10308 = CARTESIAN_POINT ( 'NONE',  ( -50.00000000000000711, -20.00000000000000000, -35.00000000000000000 ) ) ;
#10309 = CARTESIAN_POINT ( 'NONE',  ( -70.00000000000000000, 171.6227766016838245, 0.000000000000000000 ) ) ;
#10310 = CARTESIAN_POINT ( 'NONE',  ( 30.00000000000000355, 196.6227766016838245, 0.000000000000000000 ) ) ;
#10311 = LINE ( 'NONE', #17052, #14657 ) ;
#10312 = ORIENTED_EDGE ( 'NONE', *, *, #884, .T. ) ;
#10313 = EDGE_CURVE ( 'NONE', #11377, #11430, #4322, .T. ) ;
#10314 = CIRCLE ( 'NONE', #9487, 10.00000000000000178 ) ;
#10315 = CARTESIAN_POINT ( 'NONE',  ( 27.29413616237980023, 200.8416626254457356, 15.34246182976916195 ) ) ;
#10316 = ORIENTED_EDGE ( 'NONE', *, *, #8936, .T. ) ;
#10317 =( NAMED_UNIT ( * ) PLANE_ANGLE_UNIT ( ) SI_UNIT ( $, .RADIAN. ) );
#10318 = AXIS2_PLACEMENT_3D ( 'NONE', #10811, #6906, #11960 ) ;
#10319 = DIRECTION ( 'NONE',  ( 0.000000000000000000, 1.000000000000000000, 0.000000000000000000 ) ) ;
#10320 = ORIENTED_EDGE ( 'NONE', *, *, #11695, .F. ) ;
#10321 =( NAMED_UNIT ( * ) SI_UNIT ( $, .STERADIAN. ) SOLID_ANGLE_UNIT ( ) );
#10322 = DIRECTION ( 'NONE',  ( -1.000000000000000000, 0.000000000000000000, -8.673617379884037937E-17 ) ) ;
#10323 = DIRECTION ( 'NONE',  ( -1.224646799147353207E-16, -1.000000000000000000, 0.000000000000000000 ) ) ;
#10324 = CARTESIAN_POINT ( 'NONE',  ( -187.6513770290094669, 173.0877615073859772, 1.855974361197893607 ) ) ;
#10325 = FACE_OUTER_BOUND ( 'NONE', #2279, .T. ) ;
#10326 = CLOSED_SHELL ( 'NONE', ( #2846, #6764, #7644, #1401, #6214, #893, #138, #4845, #11969, #6034, #4996, #13273, #3423, #11273, #1867, #425, #11243 ) ) ;
#10327 = VECTOR ( 'NONE', #6940, 1000.000000000000000 ) ;
#10328 = ORIENTED_EDGE ( 'NONE', *, *, #16040, .T. ) ;
#10329 = DIRECTION ( 'NONE',  ( 0.000000000000000000, 0.000000000000000000, 1.000000000000000000 ) ) ;
#10330 = DIRECTION ( 'NONE',  ( -1.000000000000000000, 0.000000000000000000, -0.000000000000000000 ) ) ;
#10331 = AXIS2_PLACEMENT_3D ( 'NONE', #7132, #5459, #6955 ) ;
#10332 = CARTESIAN_POINT ( 'NONE',  ( -48.00000000000000000, 154.3022685259950038, -9.999999999999900524 ) ) ;
#10333 = SURFACE_STYLE_FILL_AREA ( #6997 ) ;
#10334 = VERTEX_POINT ( 'NONE', #72 ) ;
#10335 = EDGE_CURVE ( 'NONE', #8522, #7175, #3387, .T. ) ;
#10336 = EDGE_CURVE ( 'NONE', #7753, #7553, #4237, .T. ) ;
#10337 = EDGE_CURVE ( 'NONE', #10212, #11681, #334, .T. ) ;
#10338 = ORIENTED_EDGE ( 'NONE', *, *, #2848, .F. ) ;
#10339 = CARTESIAN_POINT ( 'NONE',  ( 17.53546816055562374, 19.99999999999999645, -24.87355917367628422 ) ) ;
#10340 = ADVANCED_FACE ( 'NONE', ( #12373 ), #10860, .F. ) ;
#10341 = CARTESIAN_POINT ( 'NONE',  ( 11.28101412774664958, 138.8108036852440250, -13.45198100927934348 ) ) ;
#10342 = ORIENTED_EDGE ( 'NONE', *, *, #11865, .T. ) ;
#10343 = DIRECTION ( 'NONE',  ( -1.000000000000000000, -0.000000000000000000, -0.000000000000000000 ) ) ;
#10344 = CARTESIAN_POINT ( 'NONE',  ( 12.56741672263938625, 143.7071609262609400, -17.59902447249972113 ) ) ;
#10345 = AXIS2_PLACEMENT_3D ( 'NONE', #12235, #16150, #13575 ) ;
#10346 = ORIENTED_EDGE ( 'NONE', *, *, #5015, .F. ) ;
#10347 = VECTOR ( 'NONE', #4108, 1000.000000000000000 ) ;
#10348 = FACE_OUTER_BOUND ( 'NONE', #12271, .T. ) ;
#10349 = DIRECTION ( 'NONE',  ( 1.000000000000000000, 0.000000000000000000, 0.000000000000000000 ) ) ;
#10350 = DIRECTION ( 'NONE',  ( -1.000000000000000000, -0.000000000000000000, 0.000000000000000000 ) ) ;
#10351 = DIRECTION ( 'NONE',  ( 0.000000000000000000, 0.000000000000000000, 1.000000000000000000 ) ) ;
#10352 = CARTESIAN_POINT ( 'NONE',  ( -12.78422937319141184, 31.72181100014091726, 11.38907491820491913 ) ) ;
#10353 = DIRECTION ( 'NONE',  ( 0.000000000000000000, 0.000000000000000000, -1.000000000000000000 ) ) ;
#10354 = AXIS2_PLACEMENT_3D ( 'NONE', #1512, #9648, #5679 ) ;
#10355 = CARTESIAN_POINT ( 'NONE',  ( 34.32861903462791986, 142.4529008285661575, -19.34799176589369907 ) ) ;
#10356 = AXIS2_PLACEMENT_3D ( 'NONE', #4003, #10715, #8139 ) ;
#10357 = VERTEX_POINT ( 'NONE', #12278 ) ;
#10358 = SPHERICAL_SURFACE ( 'NONE', #11541, 5.315148208181398104 ) ;
#10359 = CIRCLE ( 'NONE', #14051, 3.999999999999985789 ) ;
#10360 = ORIENTED_EDGE ( 'NONE', *, *, #3440, .T. ) ;
#10361 = CARTESIAN_POINT ( 'NONE',  ( -25.49999999999998579, 10.00000000000000000, 1.387778780781445676E-14 ) ) ;
#10362 = FACE_BOUND ( 'NONE', #15397, .T. ) ;
#10363 = APPLICATION_CONTEXT ( 'automotive_design' ) ;
#10364 = ORIENTED_EDGE ( 'NONE', *, *, #6527, .F. ) ;
#10365 = CARTESIAN_POINT ( 'NONE',  ( 33.88556156013721932, 19.99999999999999645, 11.42442012027869858 ) ) ;
#10366 = DIRECTION ( 'NONE',  ( -1.000000000000000000, 0.000000000000000000, 0.000000000000000000 ) ) ;
#10367 = CARTESIAN_POINT ( 'NONE',  ( 23.06881488990584472, 29.89244155294396066, 10.82591622123929653 ) ) ;
#10368 = ORIENTED_EDGE ( 'NONE', *, *, #2331, .F. ) ;
#10369 = AXIS2_PLACEMENT_3D ( 'NONE', #5578, #5671, #14958 ) ;
#10370 = CARTESIAN_POINT ( 'NONE',  ( 49.99999999999998579, 187.6227766016837961, 12.50000337241049309 ) ) ;
#10371 = CARTESIAN_POINT ( 'NONE',  ( 26.18268817859244280, 190.1433283039765172, -27.31438289289431864 ) ) ;
#10372 = CARTESIAN_POINT ( 'NONE',  ( -68.00000000000000000, 154.3022685259950038, 9.999999999999900524 ) ) ;
#10373 = CARTESIAN_POINT ( 'NONE',  ( -26.90043998675938397, 18.00000000000000000, -11.53672424425030840 ) ) ;
#10374 = EDGE_CURVE ( 'NONE', #190, #4855, #2241, .T. ) ;
#10375 = ORIENTED_EDGE ( 'NONE', *, *, #4471, .F. ) ;
#10376 = DIRECTION ( 'NONE',  ( -1.000000000000000000, -0.000000000000000000, 0.000000000000000000 ) ) ;
#10377 = EDGE_LOOP ( 'NONE', ( #11379, #27, #5434, #3717 ) ) ;
#10378 = CARTESIAN_POINT ( 'NONE',  ( 32.99829944797550496, 191.4074798671405233, -28.87243506922801473 ) ) ;
#10379 = CARTESIAN_POINT ( 'NONE',  ( -100.0000000000000000, 201.9542783778900059, -13.00000000000000000 ) ) ;
#10380 = ORIENTED_EDGE ( 'NONE', *, *, #8034, .T. ) ;
#10381 = CIRCLE ( 'NONE', #10098, 5.000000000000007994 ) ;
#10382 = ORIENTED_EDGE ( 'NONE', *, *, #2632, .T. ) ;
#10383 = ORIENTED_EDGE ( 'NONE', *, *, #3532, .T. ) ;
#10384 =( GEOMETRIC_REPRESENTATION_CONTEXT ( 3 ) GLOBAL_UNCERTAINTY_ASSIGNED_CONTEXT ( ( #15088 ) ) GLOBAL_UNIT_ASSIGNED_CONTEXT ( ( #17488, #11094, #12082 ) ) REPRESENTATION_CONTEXT ( 'NONE', 'WORKASPACE' ) );
#10385 = CIRCLE ( 'NONE', #4747, 5.000000000000004441 ) ;
#10386 = DIRECTION ( 'NONE',  ( 8.673617379884037937E-17, 0.000000000000000000, -1.000000000000000000 ) ) ;
#10387 = ORIENTED_EDGE ( 'NONE', *, *, #14471, .T. ) ;
#10388 =( NAMED_UNIT ( * ) SI_UNIT ( $, .STERADIAN. ) SOLID_ANGLE_UNIT ( ) );
#10389 = PLANE ( 'NONE',  #15280 ) ;
#10390 = DIRECTION ( 'NONE',  ( -1.000000000000000000, -0.000000000000000000, -0.000000000000000000 ) ) ;
#10391 = CARTESIAN_POINT ( 'NONE',  ( 27.57840531033536990, 152.1166601635960944, -29.06070213693891091 ) ) ;
#10392 = CARTESIAN_POINT ( 'NONE',  ( 22.65507808637627818, 17.99999999999885958, 7.619675430596801746 ) ) ;
#10393 = CARTESIAN_POINT ( 'NONE',  ( -206.3689767832464668, 166.7044760491588988, 0.5444864983987496299 ) ) ;
#10394 = EDGE_CURVE ( 'NONE', #2500, #14680, #7903, .T. ) ;
#10395 = CIRCLE ( 'NONE', #11251, 3.999999999999998668 ) ;
#10396 = ORIENTED_EDGE ( 'NONE', *, *, #8349, .F. ) ;
#10397 = CARTESIAN_POINT ( 'NONE',  ( 21.47128797932978372, 141.5899928260317040, 13.68519783011616653 ) ) ;
#10398 = DIRECTION ( 'NONE',  ( -1.000000000000000000, -6.938893903907228378E-16, 0.000000000000000000 ) ) ;
#10399 = EDGE_CURVE ( 'NONE', #10603, #15814, #12146, .T. ) ;
#10400 = CARTESIAN_POINT ( 'NONE',  ( 225.0000000000000000, 89.99999999999997158, 0.000000000000000000 ) ) ;
#10401 = CARTESIAN_POINT ( 'NONE',  ( -27.98221281347032274, 19.99999999999999645, -4.999999999999996447 ) ) ;
#10402 = VERTEX_POINT ( 'NONE', #11042 ) ;
#10403 = CARTESIAN_POINT ( 'NONE',  ( -86.42104199761078576, 142.7196187763571515, -15.94638436093396727 ) ) ;
#10404 = EDGE_CURVE ( 'NONE', #13335, #1164, #11123, .T. ) ;
#10405 = EDGE_CURVE ( 'NONE', #17378, #13903, #4513, .T. ) ;
#10406 = EDGE_CURVE ( 'NONE', #9101, #12781, #9592, .T. ) ;
#10407 = CARTESIAN_POINT ( 'NONE',  ( 30.45233391750860363, 201.6036812327912457, 13.78933345224469420 ) ) ;
#10408 = AXIS2_PLACEMENT_3D ( 'NONE', #1714, #16676, #4361 ) ;
#10409 = ORIENTED_EDGE ( 'NONE', *, *, #11865, .F. ) ;
#10410 = CARTESIAN_POINT ( 'NONE',  ( -32.66708739526796279, 101.0000000000000142, -4.722170599040662609 ) ) ;
#10412 = FACE_BOUND ( 'NONE', #14490, .T. ) ;
#10411 = VECTOR ( 'NONE', #615, 1000.000000000000000 ) ;
#10413 = ORIENTED_EDGE ( 'NONE', *, *, #625, .T. ) ;
#10414 = CARTESIAN_POINT ( 'NONE',  ( -79.53538288229906073, 141.6391889668067279, 13.78368973859834767 ) ) ;
#10415 = DIRECTION ( 'NONE',  ( 0.000000000000000000, 0.000000000000000000, -1.000000000000000000 ) ) ;
#10416 = CARTESIAN_POINT ( 'NONE',  ( -80.26436704404596867, 140.6225526278765017, -16.24764948572450507 ) ) ;
#10417 = CARTESIAN_POINT ( 'NONE',  ( 48.00000000000000711, 191.6227766016837677, -5.571800142134975431 ) ) ;
#10418 = EDGE_LOOP ( 'NONE', ( #948, #1739, #10916, #4570 ) ) ;
#10419 = DIRECTION ( 'NONE',  ( 1.000000000000000000, -0.000000000000000000, -0.000000000000000000 ) ) ;
#10420 = AXIS2_PLACEMENT_3D ( 'NONE', #10891, #5683, #5504 ) ;
#10421 = VECTOR ( 'NONE', #1241, 1000.000000000000000 ) ;
#10422 = CARTESIAN_POINT ( 'NONE',  ( 15.00000000000903455, 143.2885527162398489, 16.91661185963483760 ) ) ;
#10423 = AXIS2_PLACEMENT_3D ( 'NONE', #12265, #12446, #16352 ) ;
#10424 = FACE_BOUND ( 'NONE', #5056, .T. ) ;
#10425 = AXIS2_PLACEMENT_3D ( 'NONE', #14728, #4891, #13126 ) ;
#10426 = CARTESIAN_POINT ( 'NONE',  ( 28.59595936524185689, 202.4574374834314483, -16.55982638047048283 ) ) ;
#10427 = EDGE_LOOP ( 'NONE', ( #15343, #1519 ) ) ;
#10428 = B_SPLINE_CURVE_WITH_KNOTS ( 'NONE', 3,
 ( #13910, #14172, #4607, #8403, #4432, #4690, #10078, #1771, #9726, #13823, #8578, #12752, #11138, #12563, #11234, #1689, #7086, #8760, #620, #12486, #431, #351, #7347, #16905, #532, #7254, #13990, #16559, #1854, #14083, #8497, #15124, #5838, #11408, #12657, #705, #6018, #6099, #11330, #5751, #16654, #5938 ),
 .UNSPECIFIED., .F., .F.,
 ( 4, 2, 2, 2, 2, 2, 2, 2, 2, 2, 2, 2, 2, 2, 2, 2, 2, 2, 2, 2, 4 ),
 ( 0.000000000000000000, 0.002803867404946369657, 0.004205801107419573567, 0.005607734809892779212, 0.007009668512365983123, 0.008411602214839187033, 0.009112569066075807203, 0.009813535917312425638, 0.01051450276854904407, 0.01086498619416737324, 0.01121546961978570067, 0.01156595304540402810, 0.01191643647102235727, 0.01261740332225898438, 0.01331837017349561149, 0.01401933702473223860, 0.01542127072720551710, 0.01682320442967879734, 0.01822513813215207931, 0.01962707183462535782, 0.02243093923957190788 ),
 .UNSPECIFIED. ) ;
#10429 = VERTEX_POINT ( 'NONE', #16459 ) ;
#10430 = ORIENTED_EDGE ( 'NONE', *, *, #5159, .T. ) ;
#10431 = CARTESIAN_POINT ( 'NONE',  ( 12.52734837489390785, 131.0783166553242722, -13.12014565386486176 ) ) ;
#10432 = ORIENTED_EDGE ( 'NONE', *, *, #3323, .T. ) ;
#10433 = CARTESIAN_POINT ( 'NONE',  ( -84.82208992409042025, 150.1982800653300387, -27.67726561134452723 ) ) ;
#10434 = CARTESIAN_POINT ( 'NONE',  ( 15.42236477930291549, 143.2198172345435410, -16.80652640733168823 ) ) ;
#10435 = VECTOR ( 'NONE', #14590, 1000.000000000000000 ) ;
#10436 = VERTEX_POINT ( 'NONE', #13802 ) ;
#10437 = CYLINDRICAL_SURFACE ( 'NONE', #14354, 2.500000000000000444 ) ;
#10438 = AXIS2_PLACEMENT_3D ( 'NONE', #1436, #10887, #9393 ) ;
#10439 = DIRECTION ( 'NONE',  ( 0.000000000000000000, 0.000000000000000000, 1.000000000000000000 ) ) ;
#10440 = AXIS2_PLACEMENT_3D ( 'NONE', #11343, #11601, #3633 ) ;
#10441 = FACE_OUTER_BOUND ( 'NONE', #13539, .T. ) ;
#10442 = ADVANCED_FACE ( 'NONE', ( #15104 ), #9890, .F. ) ;
#10443 = EDGE_CURVE ( 'NONE', #14506, #16820, #13970, .T. ) ;
#10444 = EDGE_CURVE ( 'NONE', #9042, #16339, #12422, .T. ) ;
#10445 = CARTESIAN_POINT ( 'NONE',  ( -15.00000000000002132, 100.0000000000000142, 4.999999999999999112 ) ) ;
#10446 = CARTESIAN_POINT ( 'NONE',  ( 34.93420767853316988, 20.00000000000000000, 4.999999999999999112 ) ) ;
#10447 = LINE ( 'NONE', #2126, #6084 ) ;
#10448 = CARTESIAN_POINT ( 'NONE',  ( -15.50256837817153333, 32.53516993624282350, 8.343687756225392604 ) ) ;
#10449 = DIRECTION ( 'NONE',  ( 1.000000000000000000, 0.000000000000000000, 0.000000000000000000 ) ) ;
#10450 = LINE ( 'NONE', #6121, #10590 ) ;
#10451 = ORIENTED_EDGE ( 'NONE', *, *, #11915, .F. ) ;
#10452 = CARTESIAN_POINT ( 'NONE',  ( 49.99999999999998579, 163.6227766016838530, 15.00000337241049486 ) ) ;
#10453 = AXIS2_PLACEMENT_3D ( 'NONE', #1557, #2715, #12268 ) ;
#10454 = AXIS2_PLACEMENT_3D ( 'NONE', #3186, #9985, #3270 ) ;
#10455 = EDGE_LOOP ( 'NONE', ( #895, #10793, #10346, #5643 ) ) ;
#10456 = DIRECTION ( 'NONE',  ( 0.000000000000000000, 0.000000000000000000, -1.000000000000000000 ) ) ;
#10457 = VECTOR ( 'NONE', #14676, 1000.000000000000000 ) ;
#10458 = FACE_OUTER_BOUND ( 'NONE', #17301, .T. ) ;
#10459 = VERTEX_POINT ( 'NONE', #5560 ) ;
#10460 = CARTESIAN_POINT ( 'NONE',  ( -13.34744738361370509, 20.00000000000116174, 11.18154278182822026 ) ) ;
#10461 = CARTESIAN_POINT ( 'NONE',  ( 49.99999999999998579, 167.6227766016838814, 21.92820660268601074 ) ) ;
#10462 = CARTESIAN_POINT ( 'NONE',  ( 16.23563086566769442, 20.00000000000456879, 14.95434718295347665 ) ) ;
#10463 = VECTOR ( 'NONE', #12404, 1000.000000000000000 ) ;
#10464 = VERTEX_POINT ( 'NONE', #16371 ) ;
#10465 = ADVANCED_FACE ( 'NONE', ( #8382 ), #1668, .F. ) ;
#10466 = ADVANCED_FACE ( 'NONE', ( #3077 ), #12989, .F. ) ;
#10467 = CIRCLE ( 'NONE', #11322, 110.0000000000000142 ) ;
#10468 = EDGE_CURVE ( 'NONE', #6230, #16788, #14400, .T. ) ;
#10469 = CARTESIAN_POINT ( 'NONE',  ( 15.00000000000903455, 143.2885527162398489, 16.91661185963483760 ) ) ;
#10470 = CARTESIAN_POINT ( 'NONE',  ( 24.06456496986166016, 192.0313071030112155, -25.93356563065114173 ) ) ;
#10471 = DIRECTION ( 'NONE',  ( 1.000000000000000000, 0.000000000000000000, 0.000000000000000000 ) ) ;
#10472 = CARTESIAN_POINT ( 'NONE',  ( -23.66837786582113878, 18.00000000000000000, -17.32703391568840345 ) ) ;
#10473 = EDGE_LOOP ( 'NONE', ( #8557, #1675, #580, #10818 ) ) ;
#10474 = DIRECTION ( 'NONE',  ( -1.156482317317868274E-16, 1.000000000000000000, -0.000000000000000000 ) ) ;
#10475 = ORIENTED_EDGE ( 'NONE', *, *, #11462, .T. ) ;
#10476 = CARTESIAN_POINT ( 'NONE',  ( -206.3689767832464668, 174.5534660175772785, -3.987129972734268168 ) ) ;
#10477 = DIRECTION ( 'NONE',  ( -0.000000000000000000, -1.000000000000000000, 0.000000000000000000 ) ) ;
#10478 = AXIS2_PLACEMENT_3D ( 'NONE', #8511, #7268, #3112 ) ;
#10479 = ORIENTED_EDGE ( 'NONE', *, *, #5983, .F. ) ;
#10480 = VERTEX_POINT ( 'NONE', #10052 ) ;
#10481 = ORIENTED_EDGE ( 'NONE', *, *, #7115, .T. ) ;
#10482 = ADVANCED_FACE ( 'NONE', ( #3596 ), #14151, .F. ) ;
#10483 = LINE ( 'NONE', #15887, #2770 ) ;
#10484 = EDGE_LOOP ( 'NONE', ( #1911, #4069 ) ) ;
#10485 = CARTESIAN_POINT ( 'NONE',  ( 30.00000000000000711, 146.6227766016838245, -18.74999999999999645 ) ) ;
#10486 = FACE_OUTER_BOUND ( 'NONE', #17421, .T. ) ;
#10487 = CARTESIAN_POINT ( 'NONE',  ( 36.00000000000003553, 147.2627523208502964, -25.14806991105193035 ) ) ;
#10488 = VECTOR ( 'NONE', #6582, 1000.000000000000000 ) ;
#10489 = FACE_OUTER_BOUND ( 'NONE', #15457, .T. ) ;
#10490 = CARTESIAN_POINT ( 'NONE',  ( 27.48361012695488981, 138.6227766016838245, 1.225897272825924533 ) ) ;
#10491 = ORIENTED_EDGE ( 'NONE', *, *, #12091, .T. ) ;
#10492 = CARTESIAN_POINT ( 'NONE',  ( 26.01985846803728464, 139.8002605074728990, 8.764508151440994155 ) ) ;
#10493 = CARTESIAN_POINT ( 'NONE',  ( 6.134011831684049731, 144.1839557653416080, -18.33333333333335702 ) ) ;
#10494 = DIRECTION ( 'NONE',  ( 0.000000000000000000, 0.4999999999999996669, 0.8660254037844388186 ) ) ;
#10495 = CARTESIAN_POINT ( 'NONE',  ( 27.15273249069231198, 18.00000000000000000, 20.88767039909325973 ) ) ;
#10496 = CARTESIAN_POINT ( 'NONE',  ( 18.77390920412167929, 29.94862569121198348, 14.25030649093772972 ) ) ;
#10497 = ORIENTED_EDGE ( 'NONE', *, *, #2989, .T. ) ;
#10498 = CARTESIAN_POINT ( 'NONE',  ( 34.93420767853316988, 30.00000000000000000, 0.000000000000000000 ) ) ;
#10499 = CARTESIAN_POINT ( 'NONE',  ( 17.58250999373992585, 125.2198453306090329, -1.325401613797208934E-14 ) ) ;
#10500 = ORIENTED_EDGE ( 'NONE', *, *, #1385, .T. ) ;
#10501 = EDGE_CURVE ( 'NONE', #9038, #4720, #3431, .T. ) ;
#10502 = DIRECTION ( 'NONE',  ( 1.000000000000000000, 0.000000000000000000, -0.000000000000000000 ) ) ;
#10503 = CARTESIAN_POINT ( 'NONE',  ( 49.99999999999998579, 163.6227766016838530, -12.50000337241049309 ) ) ;
#10504 = ORIENTED_EDGE ( 'NONE', *, *, #12794, .T. ) ;
#10505 =( NAMED_UNIT ( * ) PLANE_ANGLE_UNIT ( ) SI_UNIT ( $, .RADIAN. ) );
#10506 = CARTESIAN_POINT ( 'NONE',  ( -27.98221281347037959, 18.00000000000000355, 0.000000000000000000 ) ) ;
#10507 = CARTESIAN_POINT ( 'NONE',  ( -45.00000000000000711, 171.6227766016838245, 0.000000000000000000 ) ) ;
#10508 = CARTESIAN_POINT ( 'NONE',  ( -74.50324869458546573, 144.1922489206527018, -21.74472059540656232 ) ) ;
#10509 = EDGE_CURVE ( 'NONE', #7894, #11405, #11569, .T. ) ;
#10510 = CARTESIAN_POINT ( 'NONE',  ( 7.743794661876905572, 133.6328069455646528, -12.86244959688548128 ) ) ;
#10511 = EDGE_CURVE ( 'NONE', #1871, #6747, #16946, .T. ) ;
#10512 = ORIENTED_EDGE ( 'NONE', *, *, #8573, .F. ) ;
#10513 = CARTESIAN_POINT ( 'NONE',  ( 48.00000000000000711, 155.6227766016839098, -10.00000337241049309 ) ) ;
#10514 = LINE ( 'NONE', #1312, #8447 ) ;
#10515 = CYLINDRICAL_SURFACE ( 'NONE', #13578, 2.499999999999998668 ) ;
#10516 = CARTESIAN_POINT ( 'NONE',  ( 37.99999999999998579, 2.000000000000000000, -28.00000000000001066 ) ) ;
#10517 = ORIENTED_EDGE ( 'NONE', *, *, #2349, .F. ) ;
#10518 = ORIENTED_EDGE ( 'NONE', *, *, #4082, .T. ) ;
#10519 = CARTESIAN_POINT ( 'NONE',  ( 7.098239199200468086, 139.5131674267937854, -14.94273745765201866 ) ) ;
#10520 = B_SPLINE_CURVE_WITH_KNOTS ( 'NONE', 3,
 ( #3938, #5516, #12068, #2775, #10904, #16155, #8254, #2607, #16236, #9407, #7992, #17377, #13398, #16328, #4194, #12241, #2511, #1361, #4028, #6767, #6922, #2860, #12163, #11976, #10653, #1266, #9577, #6672, #17477, #2687, #14732, #9231, #5247, #16059, #14984, #9321, #10552, #14810, #5346, #10745, #13583, #13663 ),
 .UNSPECIFIED., .F., .F.,
 ( 4, 2, 2, 2, 2, 2, 2, 2, 2, 2, 2, 2, 2, 2, 2, 2, 2, 2, 2, 2, 4 ),
 ( 0.000000000000000000, 0.002338598163723745824, 0.002923247704654685208, 0.003507897245585624591, 0.004677196327447558435, 0.005846495409309493581, 0.006431144950240438168, 0.007015794491171381889, 0.008185093573033232900, 0.008769743113964166212, 0.009354392654895101258, 0.01052369173675698003, 0.01110834127768790640, 0.01169299081861883277, 0.01286228990048068378, 0.01403158898234253132, 0.01461623852327344902, 0.01520088806420436672, 0.01637018714606625763, 0.01753948622792814507, 0.01870878530979003598 ),
 .UNSPECIFIED. ) ;
#10521 = ORIENTED_EDGE ( 'NONE', *, *, #16198, .T. ) ;
#10522 = DIRECTION ( 'NONE',  ( -1.000000000000000000, 0.000000000000000000, 0.000000000000000000 ) ) ;
#10523 = CARTESIAN_POINT ( 'NONE',  ( 20.41303537789175948, 141.9260521957599508, -14.39564681615556907 ) ) ;
#10524 = ORIENTED_EDGE ( 'NONE', *, *, #13344, .F. ) ;
#10525 = FACE_OUTER_BOUND ( 'NONE', #11012, .T. ) ;
#10526 = DIRECTION ( 'NONE',  ( -1.000000000000000000, 0.000000000000000000, 0.000000000000000000 ) ) ;
#10527 = CARTESIAN_POINT ( 'NONE',  ( 22.95161576004601045, 199.2315236948359143, -18.09598853029519816 ) ) ;
#10528 = CARTESIAN_POINT ( 'NONE',  ( 48.00000000000000000, 171.6227766016838245, 12.50000337241049131 ) ) ;
#10529 = DIRECTION ( 'NONE',  ( 0.000000000000000000, 1.000000000000000000, 0.000000000000000000 ) ) ;
#10530 = CARTESIAN_POINT ( 'NONE',  ( 49.99999999999998579, 191.6227766016837677, -5.571800142134975431 ) ) ;
#10531 = CARTESIAN_POINT ( 'NONE',  ( -24.99999999999999289, 90.00000000000000000, -4.999999999999999112 ) ) ;
#10532 = DIRECTION ( 'NONE',  ( 0.000000000000000000, 0.000000000000000000, 1.000000000000000000 ) ) ;
#10533 = DIRECTION ( 'NONE',  ( -1.000000000000000000, 0.000000000000000000, 0.000000000000000000 ) ) ;
#10534 = CARTESIAN_POINT ( 'NONE',  ( -45.00000000000000000, 140.0000000000000000, 15.00000000000000000 ) ) ;
#10535 = ORIENTED_EDGE ( 'NONE', *, *, #16428, .F. ) ;
#10536 = DIRECTION ( 'NONE',  ( -1.000000000000000000, -6.938893903907228378E-16, 0.000000000000000000 ) ) ;
#10537 = EDGE_LOOP ( 'NONE', ( #1180, #15630, #4222, #11815 ) ) ;
#10538 = DIRECTION ( 'NONE',  ( 1.000000000000000000, 0.000000000000000000, 0.000000000000000000 ) ) ;
#10539 = CARTESIAN_POINT ( 'NONE',  ( -7.379000772445021283, 18.00000000000000000, -25.00000000000000355 ) ) ;
#10540 = EDGE_CURVE ( 'NONE', #1367, #14130, #1123, .T. ) ;
#10541 = VERTEX_POINT ( 'NONE', #683 ) ;
#10542 = LINE ( 'NONE', #13304, #2376 ) ;
#10543 = CARTESIAN_POINT ( 'NONE',  ( 26.85584576128377066, 139.3465472469502231, 6.878002324459898453 ) ) ;
#10544 = ORIENTED_EDGE ( 'NONE', *, *, #2959, .F. ) ;
#10545 = CARTESIAN_POINT ( 'NONE',  ( 15.58467296311467898, 20.00000000000226308, 15.00881168888636807 ) ) ;
#10546 = EDGE_LOOP ( 'NONE', ( #10275, #6971, #10694, #2850 ) ) ;
#10547 = DIRECTION ( 'NONE',  ( 1.000000000000000000, 0.000000000000000000, 0.000000000000000000 ) ) ;
#10548 = CARTESIAN_POINT ( 'NONE',  ( 23.91918570238912167, 192.2260612991243818, -25.77925661938085611 ) ) ;
#10549 = CARTESIAN_POINT ( 'NONE',  ( -96.00000000000001421, 141.6227766016838245, 5.510910596163088767E-15 ) ) ;
#10550 = CARTESIAN_POINT ( 'NONE',  ( -10.72783954291835151, 17.99999999999999289, -10.92811494094397951 ) ) ;
#10551 = VERTEX_POINT ( 'NONE', #2089 ) ;
#10552 = CARTESIAN_POINT ( 'NONE',  ( 34.65073054311758938, 148.4807726931354068, 23.52860204907123887 ) ) ;
#10553 = ORIENTED_EDGE ( 'NONE', *, *, #14232, .T. ) ;
#10554 = CARTESIAN_POINT ( 'NONE',  ( -206.6026792233873550, 174.5791348918262997, -3.990824109155664878 ) ) ;
#10555 = LINE ( 'NONE', #4988, #12904 ) ;
#10556 = EDGE_CURVE ( 'NONE', #4348, #4546, #15557, .T. ) ;
#10557 = ORIENTED_EDGE ( 'NONE', *, *, #1101, .F. ) ;
#10558 = ADVANCED_FACE ( 'NONE', ( #16799 ), #13848, .T. ) ;
#10559 = ORIENTED_EDGE ( 'NONE', *, *, #1193, .T. ) ;
#10560 = ADVANCED_FACE ( 'NONE', ( #11564, #3346 ), #12732, .F. ) ;
#10561 = ORIENTED_EDGE ( 'NONE', *, *, #7117, .T. ) ;
#10562 = EDGE_CURVE ( 'NONE', #6638, #2144, #11473, .T. ) ;
#10563 = CARTESIAN_POINT ( 'NONE',  ( -75.11153254487454944, 152.3168652870156450, -26.76420670456568729 ) ) ;
#10564 = UNCERTAINTY_MEASURE_WITH_UNIT (LENGTH_MEASURE( 1.000000000000000082E-05 ), #7255, 'distance_accuracy_value', 'NONE');
#10565 = ORIENTED_EDGE ( 'NONE', *, *, #5189, .T. ) ;
#10566 = FILL_AREA_STYLE_COLOUR ( '', #11506 ) ;
#10567 = CARTESIAN_POINT ( 'NONE',  ( -16.30611068361787019, 32.76923076923078781, 4.999999999999999112 ) ) ;
#10568 = CARTESIAN_POINT ( 'NONE',  ( -15.84744341939753021, 31.82541372190370055, 11.32583567006417624 ) ) ;
#10569 = LINE ( 'NONE', #15977, #827 ) ;
#10570 = CARTESIAN_POINT ( 'NONE',  ( 33.88365274872860766, 18.00000000000000000, 11.43011099234507277 ) ) ;
#10571 = CARTESIAN_POINT ( 'NONE',  ( -84.46546100545653246, 148.8772865214095873, 23.90975478891752459 ) ) ;
#10572 = ADVANCED_BREP_SHAPE_REPRESENTATION ( '', ( #16900, #3583 ), #9837 ) ;
#10573 = VECTOR ( 'NONE', #7391, 1000.000000000000000 ) ;
#10574 = ORIENTED_EDGE ( 'NONE', *, *, #12827, .F. ) ;
#10575 = DIRECTION ( 'NONE',  ( -0.5000000000000042188, 1.060575238724903710E-16, -0.8660254037844361541 ) ) ;
#10576 = DIRECTION ( 'NONE',  ( 0.000000000000000000, 1.000000000000000000, 0.000000000000000000 ) ) ;
#10577 = CARTESIAN_POINT ( 'NONE',  ( 48.00000000000000711, 167.6227766016838530, -8.071800142134975431 ) ) ;
#10578 = CARTESIAN_POINT ( 'NONE',  ( -90.80384757729339640, 204.6227766016838245, 0.000000000000000000 ) ) ;
#10579 = CARTESIAN_POINT ( 'NONE',  ( 21.04314855419486108, 29.91877537971376455, 12.94423386069545323 ) ) ;
#10580 = EDGE_LOOP ( 'NONE', ( #1449, #2332, #15659, #7787 ) ) ;
#10581 = CARTESIAN_POINT ( 'NONE',  ( -95.00000000000000000, 171.6227766016838245, 30.00000000000000000 ) ) ;
#10582 = LINE ( 'NONE', #12993, #16975 ) ;
#10583 = ORIENTED_EDGE ( 'NONE', *, *, #10165, .T. ) ;
#10584 = FACE_OUTER_BOUND ( 'NONE', #7349, .T. ) ;
#10585 = DIRECTION ( 'NONE',  ( 1.000000000000000000, 0.000000000000000000, 0.000000000000000000 ) ) ;
#10586 = AXIS2_PLACEMENT_3D ( 'NONE', #6563, #5146, #11606 ) ;
#10587 = ORIENTED_EDGE ( 'NONE', *, *, #13621, .F. ) ;
#10588 = SURFACE_SIDE_STYLE ('',( #17239 ) ) ;
#10589 = CARTESIAN_POINT ( 'NONE',  ( -76.36134094103634595, 143.1809062453614558, 16.74061342279920339 ) ) ;
#10590 = VECTOR ( 'NONE', #10101, 1000.000000000000000 ) ;
#10591 = DIRECTION ( 'NONE',  ( -1.000000000000000000, -0.000000000000000000, -0.000000000000000000 ) ) ;
#10592 = CARTESIAN_POINT ( 'NONE',  ( -79.32805325232327220, 140.6591056634353265, -16.31724425057295136 ) ) ;
#10593 = LINE ( 'NONE', #14585, #17076 ) ;
#10594 = ORIENTED_EDGE ( 'NONE', *, *, #11523, .F. ) ;
#10595 = FACE_OUTER_BOUND ( 'NONE', #13149, .T. ) ;
#10596 = CARTESIAN_POINT ( 'NONE',  ( -73.00000000000001421, 171.6227766016838245, 0.000000000000000000 ) ) ;
#10597 = EDGE_CURVE ( 'NONE', #5655, #9695, #1926, .T. ) ;
#10598 = CARTESIAN_POINT ( 'NONE',  ( -197.9999999999999716, 171.6227766016838245, -8.000000000000007105 ) ) ;
#10599 = EDGE_CURVE ( 'NONE', #2736, #12122, #15540, .T. ) ;
#10600 = DIRECTION ( 'NONE',  ( 1.000000000000000000, 0.000000000000000000, 0.000000000000000000 ) ) ;
#10601 = AXIS2_PLACEMENT_3D ( 'NONE', #15825, #2283, #15912 ) ;
#10602 = VECTOR ( 'NONE', #15919, 1000.000000000000000 ) ;
#10603 = VERTEX_POINT ( 'NONE', #5912 ) ;
#10604 = CIRCLE ( 'NONE', #7497, 2.500000000000002220 ) ;
#10605 = ORIENTED_EDGE ( 'NONE', *, *, #16105, .T. ) ;
#10606 = CARTESIAN_POINT ( 'NONE',  ( -3.000000000000000888, 171.6227766016838245, 0.000000000000000000 ) ) ;
#10607 = ORIENTED_EDGE ( 'NONE', *, *, #1255, .F. ) ;
#10608 = CARTESIAN_POINT ( 'NONE',  ( -85.97509853867674678, 147.2612100285404040, -25.13395616064556037 ) ) ;
#10609 = EDGE_CURVE ( 'NONE', #1185, #3017, #5071, .T. ) ;
#10610 = CARTESIAN_POINT ( 'NONE',  ( 12.74723713713078155, 129.4272226793184473, -10.49625762048852451 ) ) ;
#10611 = ORIENTED_EDGE ( 'NONE', *, *, #9701, .F. ) ;
#10612 = DIRECTION ( 'NONE',  ( -1.000000000000000000, -0.000000000000000000, -0.000000000000000000 ) ) ;
#10613 = CYLINDRICAL_SURFACE ( 'NONE', #9319, 2.499999999999998668 ) ;
#10614 =( GEOMETRIC_REPRESENTATION_CONTEXT ( 3 ) GLOBAL_UNCERTAINTY_ASSIGNED_CONTEXT ( ( #15888 ) ) GLOBAL_UNIT_ASSIGNED_CONTEXT ( ( #8472, #1747, #1565 ) ) REPRESENTATION_CONTEXT ( 'NONE', 'WORKASPACE' ) );
#10615 = FACE_OUTER_BOUND ( 'NONE', #14000, .T. ) ;
#10616 = AXIS2_PLACEMENT_3D ( 'NONE', #15106, #15297, #3172 ) ;
#10617 = CARTESIAN_POINT ( 'NONE',  ( 196.0000000000000000, 191.6227766016837677, -8.071800142134975431 ) ) ;
#10618 = PLANE ( 'NONE',  #14059 ) ;
#10619 = CARTESIAN_POINT ( 'NONE',  ( 20.85766706164172035, 17.99999999999999645, -10.55326734450395954 ) ) ;
#10620 = AXIS2_PLACEMENT_3D ( 'NONE', #7265, #5949, #3460 ) ;
#10621 = CARTESIAN_POINT ( 'NONE',  ( -3.000000000000000888, 206.6227766016838245, 2.143131898507868248E-15 ) ) ;
#10622 = PLANE ( 'NONE',  #543 ) ;
#10623 = CARTESIAN_POINT ( 'NONE',  ( 34.93420767853316988, 30.00000000000000000, -15.00000000000000000 ) ) ;
#10624 = EDGE_CURVE ( 'NONE', #13611, #8809, #604, .T. ) ;
#10625 = DIRECTION ( 'NONE',  ( 1.000000000000000000, 0.000000000000000000, -0.000000000000000000 ) ) ;
#10626 = VERTEX_POINT ( 'NONE', #2177 ) ;
#10627 = CARTESIAN_POINT ( 'NONE',  ( -25.00000000000002132, 120.0000000000000284, -5.000000000000023093 ) ) ;
#10628 = CARTESIAN_POINT ( 'NONE',  ( -19.25702671965661850, 19.99999999999999645, -21.36300512502526416 ) ) ;
#10629 = VERTEX_POINT ( 'NONE', #15632 ) ;
#10630 = DIRECTION ( 'NONE',  ( -1.000000000000000000, 0.000000000000000000, 0.000000000000000000 ) ) ;
#10631 = AXIS2_PLACEMENT_3D ( 'NONE', #5449, #13597, #3043 ) ;
#10632 = EDGE_CURVE ( 'NONE', #7474, #9334, #10153, .T. ) ;
#10633 = CARTESIAN_POINT ( 'NONE',  ( -73.00000000000001421, 171.6227766016838245, 19.49999999999998934 ) ) ;
#10634 = CIRCLE ( 'NONE', #13473, 30.00000000000000000 ) ;
#10635 = ORIENTED_EDGE ( 'NONE', *, *, #15550, .T. ) ;
#10636 = EDGE_CURVE ( 'NONE', #15924, #1583, #8989, .T. ) ;
#10637 = CARTESIAN_POINT ( 'NONE',  ( -8.097611523674038025, 19.99999999997653788, 14.83628426572619219 ) ) ;
#10638 = EDGE_CURVE ( 'NONE', #9170, #6523, #11997, .T. ) ;
#10639 = CARTESIAN_POINT ( 'NONE',  ( 15.45419697039644902, 125.5863960662987040, 6.086967932831932160 ) ) ;
#10640 = ORIENTED_EDGE ( 'NONE', *, *, #320, .F. ) ;
#10641 = CARTESIAN_POINT ( 'NONE',  ( 18.47379060770018810, 20.00000000000225953, 14.40819024183099728 ) ) ;
#10642 = VERTEX_POINT ( 'NONE', #10493 ) ;
#10643 = CARTESIAN_POINT ( 'NONE',  ( -98.00000000000000000, 171.6227766016838245, 0.000000000000000000 ) ) ;
#10644 = AXIS2_PLACEMENT_3D ( 'NONE', #11241, #16912, #8926 ) ;
#10645 = AXIS2_PLACEMENT_3D ( 'NONE', #6370, #11676, #13288 ) ;
#10646 = CARTESIAN_POINT ( 'NONE',  ( 26.92553734538028110, 189.7763206329742047, -27.55849099911373301 ) ) ;
#10647 = DIRECTION ( 'NONE',  ( -1.000000000000000000, -0.000000000000000000, -0.000000000000000000 ) ) ;
#10648 = EDGE_CURVE ( 'NONE', #5870, #2623, #13247, .T. ) ;
#10649 = AXIS2_PLACEMENT_3D ( 'NONE', #6558, #4002, #5 ) ;
#10650 = CARTESIAN_POINT ( 'NONE',  ( -15.50256837817153333, 32.53516993624282350, -8.343687756225392604 ) ) ;
#10651 = CIRCLE ( 'NONE', #6398, 2.500000000000002220 ) ;
#10652 = EDGE_LOOP ( 'NONE', ( #13129, #2652 ) ) ;
#10653 = CARTESIAN_POINT ( 'NONE',  ( 31.52945631074817356, 151.3869516943736357, 26.06757126999134755 ) ) ;
#10654 = ORIENTED_EDGE ( 'NONE', *, *, #8341, .T. ) ;
#10655 = CARTESIAN_POINT ( 'NONE',  ( -80.59986690501729356, 189.1412428432857951, -27.96613953460097690 ) ) ;
#10656 = DIRECTION ( 'NONE',  ( 0.000000000000000000, 0.000000000000000000, 1.000000000000000000 ) ) ;
#10657 = VERTEX_POINT ( 'NONE', #2437 ) ;
#10658 = ORIENTED_EDGE ( 'NONE', *, *, #6556, .T. ) ;
#10659 = ORIENTED_EDGE ( 'NONE', *, *, #4185, .T. ) ;
#10660 = CIRCLE ( 'NONE', #14072, 1.000000000000000888 ) ;
#10661 = CARTESIAN_POINT ( 'NONE',  ( 15.00000000000000000, 206.6227766016838245, -2.143131898507868248E-15 ) ) ;
#10662 = VERTEX_POINT ( 'NONE', #9252 ) ;
#10663 = CARTESIAN_POINT ( 'NONE',  ( 15.58935622847965163, 125.0306600298041815, -3.338394242842863679 ) ) ;
#10664 = SURFACE_SIDE_STYLE ('',( #1110 ) ) ;
#10665 = CARTESIAN_POINT ( 'NONE',  ( 25.29742550462585982, 150.3543615375533022, -27.79730406782767105 ) ) ;
#10666 = EDGE_CURVE ( 'NONE', #10091, #15177, #5444, .T. ) ;
#10667 = LINE ( 'NONE', #8006, #11047 ) ;
#10668 = ADVANCED_FACE ( 'NONE', ( #15810 ), #6328, .F. ) ;
#10669 = CARTESIAN_POINT ( 'NONE',  ( -81.91034726766426388, 151.2585272520459512, 25.96811968750270339 ) ) ;
#10670 = EDGE_CURVE ( 'NONE', #11875, #16488, #6076, .T. ) ;
#10671 = EDGE_LOOP ( 'NONE', ( #11807, #15798, #7561, #10832 ) ) ;
#10672 = CARTESIAN_POINT ( 'NONE',  ( -83.47514333733060710, 201.5283731665715834, -18.18938113080313101 ) ) ;
#10673 = CARTESIAN_POINT ( 'NONE',  ( 23.61565302391275267, 29.88537503463918554, -10.00682404417760551 ) ) ;
#10674 = AXIS2_PLACEMENT_3D ( 'NONE', #4063, #9533, #14937 ) ;
#10675 = CARTESIAN_POINT ( 'NONE',  ( 16.69631138515844171, 126.9345490261019904, 8.565329098038530375 ) ) ;
#10676 = AXIS2_PLACEMENT_3D ( 'NONE', #3587, #5089, #5001 ) ;
#10677 = CARTESIAN_POINT ( 'NONE',  ( 37.99999999999998579, 20.00000000000000000, -30.00000000000001066 ) ) ;
#10678 = DIRECTION ( 'NONE',  ( -2.312964634635742464E-16, 0.000000000000000000, -1.000000000000000000 ) ) ;
#10679 = ORIENTED_EDGE ( 'NONE', *, *, #15423, .F. ) ;
#10680 = LINE ( 'NONE', #10771, #8356 ) ;
#10681 = VECTOR ( 'NONE', #214, 1000.000000000000000 ) ;
#10682 = CARTESIAN_POINT ( 'NONE',  ( -40.00000000000000000, 20.00000000000000000, 30.00000000000000355 ) ) ;
#10683 = LINE ( 'NONE', #5547, #9329 ) ;
#10684 = EDGE_LOOP ( 'NONE', ( #5133, #7708 ) ) ;
#10685 = SURFACE_STYLE_FILL_AREA ( #2449 ) ;
#10686 = EDGE_LOOP ( 'NONE', ( #14775, #4035 ) ) ;
#10687 = SHAPE_REPRESENTATION_RELATIONSHIP ( 'NONE' , 'NONE' ,  #690, #12908 ) ;
#10688 = AXIS2_PLACEMENT_3D ( 'NONE', #6400, #16953, #3749 ) ;
#10689 = MECHANICAL_DESIGN_GEOMETRIC_PRESENTATION_REPRESENTATION (  '', ( #2787 ), #16069 ) ;
#10690 = CARTESIAN_POINT ( 'NONE',  ( 15.45427063382542165, 18.00000000000226663, -13.01057400152831711 ) ) ;
#10691 = CARTESIAN_POINT ( 'NONE',  ( -82.40346994510062473, 141.1206502181308622, -17.16533225383573935 ) ) ;
#10692 = EDGE_CURVE ( 'NONE', #5017, #11907, #6423, .T. ) ;
#10693 = DIRECTION ( 'NONE',  ( -1.000000000000000000, -0.000000000000000000, 0.000000000000000000 ) ) ;
#10694 = ORIENTED_EDGE ( 'NONE', *, *, #6492, .T. ) ;
#10695 = CARTESIAN_POINT ( 'NONE',  ( -725.0000000000000000, 19.99999999999995737, 13.00000000000000000 ) ) ;
#10696 = CARTESIAN_POINT ( 'NONE',  ( 11.38015211399644500, 143.8700659084811093, 17.85516819212570638 ) ) ;
#10697 = CARTESIAN_POINT ( 'NONE',  ( -27.99999999999998224, 10.00000000000000000, -16.00000000000000000 ) ) ;
#10698 = FACE_BOUND ( 'NONE', #15566, .T. ) ;
#10699 = AXIS2_PLACEMENT_3D ( 'NONE', #11833, #17329, #16104 ) ;
#10700 = EDGE_LOOP ( 'NONE', ( #14475, #4181, #14216, #2931 ) ) ;
#10701 = CARTESIAN_POINT ( 'NONE',  ( 9.819856892917396607, 139.1316717379867214, -14.17181165802795206 ) ) ;
#10702 = VERTEX_POINT ( 'NONE', #17501 ) ;
#10703 = LINE ( 'NONE', #15752, #11494 ) ;
#10704 = CARTESIAN_POINT ( 'NONE',  ( 14.24850047812951104, 138.6393229685333779, -3.919138222309428876 ) ) ;
#10705 = VERTEX_POINT ( 'NONE', #10766 ) ;
#10706 = DIRECTION ( 'NONE',  ( -1.000000000000000000, 0.000000000000000000, 0.000000000000000000 ) ) ;
#10707 = CARTESIAN_POINT ( 'NONE',  ( -206.3689767832464668, 216.7416069248773169, -29.43343747897081286 ) ) ;
#10708 = EDGE_CURVE ( 'NONE', #15255, #2414, #7834, .T. ) ;
#10709 = CYLINDRICAL_SURFACE ( 'NONE', #15490, 4.750000000000000000 ) ;
#10710 = CIRCLE ( 'NONE', #2226, 2.500000000000002220 ) ;
#10711 = APPLICATION_CONTEXT ( 'automotive_design' ) ;
#10712 = AXIS2_PLACEMENT_3D ( 'NONE', #5719, #3229, #15275 ) ;
#10713 = CARTESIAN_POINT ( 'NONE',  ( 35.00000000000001421, 196.3674529106260707, 21.83698684826044101 ) ) ;
#10714 = AXIS2_PLACEMENT_3D ( 'NONE', #7229, #8892, #3340 ) ;
#10715 = DIRECTION ( 'NONE',  ( -1.000000000000000000, -0.000000000000000000, -0.000000000000000000 ) ) ;
#10716 = CARTESIAN_POINT ( 'NONE',  ( 21.44211297938456084, 29.87092986353274426, -9.660732976998257726 ) ) ;
#10717 = FACE_OUTER_BOUND ( 'NONE', #12232, .T. ) ;
#10718 = CARTESIAN_POINT ( 'NONE',  ( -192.9999999999999716, 171.6227766016838245, -14.16444493696511486 ) ) ;
#10719 = CARTESIAN_POINT ( 'NONE',  ( 35.00000000000000000, 196.6227766016838245, 0.000000000000000000 ) ) ;
#10720 = FACE_OUTER_BOUND ( 'NONE', #3330, .T. ) ;
#10721 = VERTEX_POINT ( 'NONE', #5371 ) ;
#10722 = DIRECTION ( 'NONE',  ( 0.000000000000000000, 0.000000000000000000, 1.000000000000000000 ) ) ;
#10723 = ORIENTED_EDGE ( 'NONE', *, *, #3100, .T. ) ;
#10724 = CARTESIAN_POINT ( 'NONE',  ( 39.99999999999998579, 0.000000000000000000, -33.00000000000000711 ) ) ;
#10725 = AXIS2_PLACEMENT_3D ( 'NONE', #509, #12812, #6001 ) ;
#10726 = CARTESIAN_POINT ( 'NONE',  ( -45.00000000000000000, 122.0000000000000142, 0.000000000000000000 ) ) ;
#10727 = CIRCLE ( 'NONE', #834, 14.16444493696511486 ) ;
#10728 = EDGE_LOOP ( 'NONE', ( #7401, #16004, #1483, #5167, #5136, #14811, #16240 ) ) ;
#10729 = CARTESIAN_POINT ( 'NONE',  ( -10.87333020471588974, 20.00000000000114753, 13.51515657978521645 ) ) ;
#10730 = AXIS2_PLACEMENT_3D ( 'NONE', #2868, #5873, #5706 ) ;
#10731 = CARTESIAN_POINT ( 'NONE',  ( 14.12560798726494760, 138.8049619564753243, 7.597757983846928020 ) ) ;
#10732 = VERTEX_POINT ( 'NONE', #3768 ) ;
#10733 = CARTESIAN_POINT ( 'NONE',  ( 17.68052782483612617, 29.96314637258912583, 14.61659083303745632 ) ) ;
#10734 = EDGE_CURVE ( 'NONE', #2144, #15700, #5009, .T. ) ;
#10735 = EDGE_LOOP ( 'NONE', ( #4195, #14390 ) ) ;
#10736 = LINE ( 'NONE', #4100, #4711 ) ;
#10737 = DIRECTION ( 'NONE',  ( 0.000000000000000000, 0.000000000000000000, 1.000000000000000000 ) ) ;
#10738 = CIRCLE ( 'NONE', #586, 20.00000000000000355 ) ;
#10739 = LINE ( 'NONE', #11884, #10214 ) ;
#10740 = CARTESIAN_POINT ( 'NONE',  ( -80.00000000000001421, 196.6227766016838245, -16.00000000000000000 ) ) ;
#10741 = EDGE_CURVE ( 'NONE', #15996, #6096, #9159, .T. ) ;
#10742 = VECTOR ( 'NONE', #16987, 1000.000000000000000 ) ;
#10743 = ADVANCED_FACE ( 'NONE', ( #14568 ), #6518, .T. ) ;
#10744 = ORIENTED_EDGE ( 'NONE', *, *, #6448, .F. ) ;
#10745 = CARTESIAN_POINT ( 'NONE',  ( 34.98058807492896705, 147.1381844727102646, 22.12819033745955011 ) ) ;
#10746 = VERTEX_POINT ( 'NONE', #5183 ) ;
#10747 = DIRECTION ( 'NONE',  ( 0.000000000000000000, 0.000000000000000000, -1.000000000000000000 ) ) ;
#10748 = DIRECTION ( 'NONE',  ( 1.000000000000000000, 0.000000000000000000, 0.000000000000000000 ) ) ;
#10749 = EDGE_LOOP ( 'NONE', ( #14368, #7495, #15231, #9566 ) ) ;
#10750 = VERTEX_POINT ( 'NONE', #5960 ) ;
#10751 = EDGE_LOOP ( 'NONE', ( #7860, #4831, #1678, #11556 ) ) ;
#10752 = AXIS2_PLACEMENT_3D ( 'NONE', #15452, #10366, #5898 ) ;
#10753 = VECTOR ( 'NONE', #2539, 1000.000000000000000 ) ;
#10754 = CARTESIAN_POINT ( 'NONE',  ( 9.819856892917396607, 139.1316717379867214, 14.17181165802734988 ) ) ;
#10755 = CIRCLE ( 'NONE', #3120, 35.00000000000000000 ) ;
#10756 = ORIENTED_EDGE ( 'NONE', *, *, #16605, .F. ) ;
#10757 = CONTEXT_DEPENDENT_SHAPE_REPRESENTATION ( #14898, #513 ) ;
#10758 = CARTESIAN_POINT ( 'NONE',  ( 6.134011831684053284, 142.5209969267753820, -19.44444444444444642 ) ) ;
#10759 = DIRECTION ( 'NONE',  ( -1.000000000000000000, 0.000000000000000000, 0.000000000000000000 ) ) ;
#10760 = CARTESIAN_POINT ( 'NONE',  ( -22.99999999999999289, 120.0000000000000142, 0.000000000000000000 ) ) ;
#10761 = CYLINDRICAL_SURFACE ( 'NONE', #1722, 19.49999999999999645 ) ;
#10762 = CARTESIAN_POINT ( 'NONE',  ( -75.68194015699739907, 149.1480937705748602, 24.16447509748838485 ) ) ;
#10763 = ORIENTED_EDGE ( 'NONE', *, *, #7209, .F. ) ;
#10764 = DIRECTION ( 'NONE',  ( -1.000000000000000000, 0.000000000000000000, 0.000000000000000000 ) ) ;
#10765 = AXIS2_PLACEMENT_3D ( 'NONE', #17359, #751, #5231 ) ;
#10766 = CARTESIAN_POINT ( 'NONE',  ( 49.99999999999998579, 179.6227766016838245, 15.00000337241049486 ) ) ;
#10767 = CARTESIAN_POINT ( 'NONE',  ( -155.0000000000000284, 171.6227766016838245, 0.000000000000000000 ) ) ;
#10768 = CARTESIAN_POINT ( 'NONE',  ( 16.25302816831168329, 18.00000000000000000, 25.00000000000000000 ) ) ;
#10769 = AXIS2_PLACEMENT_3D ( 'NONE', #5878, #15167, #8444 ) ;
#10770 = FACE_OUTER_BOUND ( 'NONE', #15383, .T. ) ;
#10771 = CARTESIAN_POINT ( 'NONE',  ( -15.00000000000002132, 90.00000000000000000, 15.00000000000000000 ) ) ;
#10772 = SHAPE_REPRESENTATION ( 'gear selector switch', ( #3583 ), #3025 ) ;
#10773 = CARTESIAN_POINT ( 'NONE',  ( -80.00000000000001421, 196.6227766016838245, 0.000000000000000000 ) ) ;
#10774 = EDGE_CURVE ( 'NONE', #5721, #5744, #15414, .T. ) ;
#10775 = ORIENTED_EDGE ( 'NONE', *, *, #16534, .F. ) ;
#10776 = AXIS2_PLACEMENT_3D ( 'NONE', #4980, #1088, #14459 ) ;
#10777 = EDGE_LOOP ( 'NONE', ( #16589, #10475, #2517, #14403 ) ) ;
#10778 = SURFACE_STYLE_FILL_AREA ( #9615 ) ;
#10779 = DIRECTION ( 'NONE',  ( 0.000000000000000000, 0.000000000000000000, 1.000000000000000000 ) ) ;
#10780 = CARTESIAN_POINT ( 'NONE',  ( -23.00000000000002132, 122.0000000000000142, -9.686291501015228178 ) ) ;
#10781 = CARTESIAN_POINT ( 'NONE',  ( -84.78365660347692767, 142.9837419059134334, -20.12545249291982330 ) ) ;
#10782 = FACE_OUTER_BOUND ( 'NONE', #15906, .T. ) ;
#10783 = EDGE_LOOP ( 'NONE', ( #13984, #6837 ) ) ;
#10784 = DIRECTION ( 'NONE',  ( 1.000000000000000000, 0.000000000000000000, 0.000000000000000000 ) ) ;
#10785 = CARTESIAN_POINT ( 'NONE',  ( -207.9328752093750836, 173.0003187169972989, -5.418902083281068371 ) ) ;
#10786 = DIRECTION ( 'NONE',  ( -0.000000000000000000, -0.000000000000000000, -1.000000000000000000 ) ) ;
#10787 = AXIS2_PLACEMENT_3D ( 'NONE', #17293, #9403, #31 ) ;
#10788 = ORIENTED_EDGE ( 'NONE', *, *, #15816, .F. ) ;
#10789 = CARTESIAN_POINT ( 'NONE',  ( 48.00000000000000711, 175.6227766016838245, -8.071800142134975431 ) ) ;
#10790 = EDGE_CURVE ( 'NONE', #9609, #5289, #12286, .T. ) ;
#10791 = EDGE_CURVE ( 'NONE', #1100, #7583, #7482, .T. ) ;
#10792 = EDGE_CURVE ( 'NONE', #6881, #5246, #15968, .T. ) ;
#10793 = ORIENTED_EDGE ( 'NONE', *, *, #13086, .F. ) ;
#10794 = DIRECTION ( 'NONE',  ( 0.000000000000000000, -1.000000000000000000, 0.000000000000000000 ) ) ;
#10795 = DIRECTION ( 'NONE',  ( -1.000000000000000000, -0.000000000000000000, 0.000000000000000000 ) ) ;
#10796 = ORIENTED_EDGE ( 'NONE', *, *, #1422, .T. ) ;
#10797 = CARTESIAN_POINT ( 'NONE',  ( -22.99999999999998224, 10.00000000000000000, 0.000000000000000000 ) ) ;
#10798 = CARTESIAN_POINT ( 'NONE',  ( -27.99999999999998224, 10.00000000000000000, 0.000000000000000000 ) ) ;
#10799 = DIRECTION ( 'NONE',  ( -0.08715574274764655016, -0.4980973490458782127, 0.8627299156628190913 ) ) ;
#10800 = CARTESIAN_POINT ( 'NONE',  ( 48.00000000000000711, 187.6227766016837961, 15.00000337241049486 ) ) ;
#10801 = DIRECTION ( 'NONE',  ( -1.000000000000000000, 0.000000000000000000, 0.000000000000000000 ) ) ;
#10802 = CARTESIAN_POINT ( 'NONE',  ( 18.97220464449422295, 17.99999999999999645, -12.00279687791388383 ) ) ;
#10803 = DIRECTION ( 'NONE',  ( 0.000000000000000000, 0.000000000000000000, 1.000000000000000000 ) ) ;
#10804 = CARTESIAN_POINT ( 'NONE',  ( -80.00000000000001421, 196.6227766016838245, -35.00000000000000000 ) ) ;
#10805 = FACE_OUTER_BOUND ( 'NONE', #7239, .T. ) ;
#10806 = DIRECTION ( 'NONE',  ( -1.000000000000000000, 0.000000000000000000, 0.000000000000000000 ) ) ;
#10807 = VERTEX_POINT ( 'NONE', #9749 ) ;
#10808 = DIRECTION ( 'NONE',  ( -1.000000000000000000, 0.000000000000000000, 0.000000000000000000 ) ) ;
#10809 = ORIENTED_EDGE ( 'NONE', *, *, #987, .T. ) ;
#10810 = EDGE_CURVE ( 'NONE', #4487, #2548, #8325, .T. ) ;
#10811 = CARTESIAN_POINT ( 'NONE',  ( -45.00000000000000711, 8.000000000000000000, -35.00000000000000000 ) ) ;
#10812 = CARTESIAN_POINT ( 'NONE',  ( 196.0000000000000000, 159.6227766016838814, 5.571800142134975431 ) ) ;
#10813 = ORIENTED_EDGE ( 'NONE', *, *, #10151, .F. ) ;
#10814 = CARTESIAN_POINT ( 'NONE',  ( -13.66886994730069560, 31.37497952739824214, 13.17845503416513075 ) ) ;
#10815 = CARTESIAN_POINT ( 'NONE',  ( 13.54862175821475034, 128.4555333983033734, 9.713103375557215813 ) ) ;
#10816 = ORIENTED_EDGE ( 'NONE', *, *, #1855, .T. ) ;
#10817 = CARTESIAN_POINT ( 'NONE',  ( 20.11141720500585350, 19.99999999999999645, 24.32074799214527516 ) ) ;
#10818 = ORIENTED_EDGE ( 'NONE', *, *, #2506, .T. ) ;
#10819 = CARTESIAN_POINT ( 'NONE',  ( -116.4755503550297107, 171.6227766016838245, 0.000000000000000000 ) ) ;
#10820 = LINE ( 'NONE', #194, #8902 ) ;
#10821 = DIRECTION ( 'NONE',  ( 0.000000000000000000, 1.000000000000000000, 0.000000000000000000 ) ) ;
#10822 = DIRECTION ( 'NONE',  ( 0.000000000000000000, 0.000000000000000000, 1.000000000000000000 ) ) ;
#10823 = ORIENTED_EDGE ( 'NONE', *, *, #847, .F. ) ;
#10824 = CYLINDRICAL_SURFACE ( 'NONE', #8435, 2.500000000000002220 ) ;
#10825 = EDGE_CURVE ( 'NONE', #4808, #16973, #14549, .T. ) ;
#10826 = ORIENTED_EDGE ( 'NONE', *, *, #843, .F. ) ;
#10827 = ADVANCED_FACE ( 'NONE', ( #370 ), #3245, .F. ) ;
#10828 = CARTESIAN_POINT ( 'NONE',  ( -75.75320729262173813, 190.4349707265699294, -27.11332964807919765 ) ) ;
#10829 = DIRECTION ( 'NONE',  ( -0.000000000000000000, -0.000000000000000000, -1.000000000000000000 ) ) ;
#10830 = VERTEX_POINT ( 'NONE', #1880 ) ;
#10831 = ORIENTED_EDGE ( 'NONE', *, *, #5157, .F. ) ;
#10832 = ORIENTED_EDGE ( 'NONE', *, *, #14371, .F. ) ;
#10833 = CARTESIAN_POINT ( 'NONE',  ( -7.379000772445021283, 30.00000000000000000, -13.00000000000000000 ) ) ;
#10834 = EDGE_CURVE ( 'NONE', #6096, #817, #5771, .T. ) ;
#10835 = ORIENTED_EDGE ( 'NONE', *, *, #7314, .T. ) ;
#10836 = SHAPE_DEFINITION_REPRESENTATION ( #4477, #13460 ) ;
#10837 = DIRECTION ( 'NONE',  ( -1.000000000000000000, 0.000000000000000000, 0.000000000000000000 ) ) ;
#10838 = DIRECTION ( 'NONE',  ( -1.000000000000000000, 0.000000000000000000, 0.000000000000000000 ) ) ;
#10839 = CARTESIAN_POINT ( 'NONE',  ( -40.00000000000000000, 20.00000000000000000, 30.00000000000000355 ) ) ;
#10840 = CARTESIAN_POINT ( 'NONE',  ( -80.00000000000002842, 146.6227766016838245, 0.000000000000000000 ) ) ;
#10841 = CARTESIAN_POINT ( 'NONE',  ( -79.62047275650606082, 151.6237922324447993, 26.24958334688937711 ) ) ;
#10842 = ORIENTED_EDGE ( 'NONE', *, *, #14418, .T. ) ;
#10843 = CARTESIAN_POINT ( 'NONE',  ( -78.93349828499714249, 202.5285685493726362, -16.42664996635052432 ) ) ;
#10844 = LINE ( 'NONE', #2710, #10753 ) ;
#10845 = CARTESIAN_POINT ( 'NONE',  ( 33.66231827095856488, 20.00000000000000000, -12.04861179558545636 ) ) ;
#10846 = CARTESIAN_POINT ( 'NONE',  ( -207.2467692809709376, 173.4734229514064339, 4.797581375662468339 ) ) ;
#10847 = DIRECTION ( 'NONE',  ( 1.000000000000000000, 0.000000000000000000, 0.000000000000000000 ) ) ;
#10848 = FACE_OUTER_BOUND ( 'NONE', #196, .T. ) ;
#10849 = ORIENTED_EDGE ( 'NONE', *, *, #11223, .T. ) ;
#10850 = CARTESIAN_POINT ( 'NONE',  ( 30.00000000000000355, 196.6227766016838245, 10.00000000000000178 ) ) ;
#10851 = EDGE_CURVE ( 'NONE', #1349, #11959, #17385, .T. ) ;
#10852 = ORIENTED_EDGE ( 'NONE', *, *, #6293, .T. ) ;
#10853 = CARTESIAN_POINT ( 'NONE',  ( 24.00000000000000000, 196.6227766016838245, -24.49489742783178770 ) ) ;
#10854 = DIRECTION ( 'NONE',  ( 1.000000000000000000, 0.000000000000000000, 0.000000000000000000 ) ) ;
#10855 = DIRECTION ( 'NONE',  ( 0.000000000000000000, 0.000000000000000000, -1.000000000000000000 ) ) ;
#10856 = CIRCLE ( 'NONE', #4691, 33.00000000000000000 ) ;
#10857 = DIRECTION ( 'NONE',  ( -1.000000000000000000, 0.000000000000000000, 0.000000000000000000 ) ) ;
#10858 = ORIENTED_EDGE ( 'NONE', *, *, #7036, .T. ) ;
#10859 = DIRECTION ( 'NONE',  ( 0.000000000000000000, 0.000000000000000000, -1.000000000000000000 ) ) ;
#10860 = CYLINDRICAL_SURFACE ( 'NONE', #7052, 2.499999999999998668 ) ;
#10861 = EDGE_CURVE ( 'NONE', #12804, #8947, #9930, .T. ) ;
#10862 = CYLINDRICAL_SURFACE ( 'NONE', #2267, 5.000000000000004441 ) ;
#10863 = AXIS2_PLACEMENT_3D ( 'NONE', #3869, #2540, #13339 ) ;
#10864 = CARTESIAN_POINT ( 'NONE',  ( 15.51497662817079082, 137.3737080369936905, -9.118346648348486738 ) ) ;
#10865 = AXIS2_PLACEMENT_3D ( 'NONE', #10534, #10625, #15941 ) ;
#10866 = ORIENTED_EDGE ( 'NONE', *, *, #7335, .T. ) ;
#10867 = DIRECTION ( 'NONE',  ( 1.000000000000000000, 0.000000000000000000, 0.000000000000000000 ) ) ;
#10868 = CARTESIAN_POINT ( 'NONE',  ( -22.99999999999999289, 100.0000000000000142, 0.000000000000000000 ) ) ;
#10869 = VERTEX_POINT ( 'NONE', #5692 ) ;
#10870 = CARTESIAN_POINT ( 'NONE',  ( -80.21954352204551242, 190.6224931067073953, -29.39406016266899968 ) ) ;
#10871 = CARTESIAN_POINT ( 'NONE',  ( -208.1430079281944074, 169.2505655449146786, 4.108790076600837615 ) ) ;
#10872 = DIRECTION ( 'NONE',  ( -1.000000000000000000, -0.000000000000000000, -0.000000000000000000 ) ) ;
#10873 = CARTESIAN_POINT ( 'NONE',  ( 34.42405209918207731, 18.00000000000000000, -9.535225002503356251 ) ) ;
#10874 = CIRCLE ( 'NONE', #12579, 747.9999999999998863 ) ;
#10875 = CARTESIAN_POINT ( 'NONE',  ( 23.18512258076444610, 18.00000000000000000, -23.22991426836919615 ) ) ;
#10876 = DIRECTION ( 'NONE',  ( -1.000000000000000000, 0.000000000000000000, 0.000000000000000000 ) ) ;
#10877 = DIRECTION ( 'NONE',  ( 1.000000000000000000, 0.000000000000000000, 0.000000000000000000 ) ) ;
#10878 = EDGE_CURVE ( 'NONE', #8582, #15415, #11154, .T. ) ;
#10879 = EDGE_CURVE ( 'NONE', #16992, #1871, #16495, .T. ) ;
#10880 = MECHANICAL_DESIGN_GEOMETRIC_PRESENTATION_REPRESENTATION (  '', ( #11453 ), #16269 ) ;
#10881 = FACE_OUTER_BOUND ( 'NONE', #495, .T. ) ;
#10882 = ADVANCED_FACE ( 'NONE', ( #11160 ), #8427, .T. ) ;
#10883 = DIRECTION ( 'NONE',  ( -0.000000000000000000, -0.000000000000000000, -1.000000000000000000 ) ) ;
#10884 = ORIENTED_EDGE ( 'NONE', *, *, #3059, .T. ) ;
#10885 = CARTESIAN_POINT ( 'NONE',  ( -70.00000000000000000, 171.6227766016838245, 0.000000000000000000 ) ) ;
#10886 = ORIENTED_EDGE ( 'NONE', *, *, #17264, .T. ) ;
#10887 = DIRECTION ( 'NONE',  ( -1.000000000000000000, 0.000000000000000000, -2.312964634635742464E-16 ) ) ;
#10888 = DIRECTION ( 'NONE',  ( -0.000000000000000000, -0.000000000000000000, 1.000000000000000000 ) ) ;
#10889 = ORIENTED_EDGE ( 'NONE', *, *, #10394, .T. ) ;
#10890 = CARTESIAN_POINT ( 'NONE',  ( 1.559999999999998943, -1.732050807568885631, 0.000000000000000000 ) ) ;
#10891 = CARTESIAN_POINT ( 'NONE',  ( 48.00000000000000711, 151.6227766016839098, -5.571800142134973655 ) ) ;
#10892 = ORIENTED_EDGE ( 'NONE', *, *, #8829, .T. ) ;
#10893 = AXIS2_PLACEMENT_3D ( 'NONE', #13702, #16462, #13972 ) ;
#10894 = CARTESIAN_POINT ( 'NONE',  ( 31.45415618582128658, 153.9859494455611468, -27.89172594985638653 ) ) ;
#10895 = AXIS2_PLACEMENT_3D ( 'NONE', #627, #1693, #7351 ) ;
#10896 = VERTEX_POINT ( 'NONE', #13745 ) ;
#10897 = LINE ( 'NONE', #6845, #9224 ) ;
#10898 = CARTESIAN_POINT ( 'NONE',  ( 32.50000000000000000, 196.6227766016838245, 0.000000000000000000 ) ) ;
#10899 = DIRECTION ( 'NONE',  ( -1.000000000000000000, 0.000000000000000000, 0.000000000000000000 ) ) ;
#10900 = VERTEX_POINT ( 'NONE', #1789 ) ;
#10901 = CARTESIAN_POINT ( 'NONE',  ( 30.00000000000001066, 146.6227766016838245, 35.00200000000000244 ) ) ;
#10902 = CIRCLE ( 'NONE', #15705, 2.500000000000002220 ) ;
#10903 = VERTEX_POINT ( 'NONE', #11080 ) ;
#10904 = CARTESIAN_POINT ( 'NONE',  ( 25.35214468288316070, 148.4718376841440204, 23.51742847763245337 ) ) ;
#10905 = AXIS2_PLACEMENT_3D ( 'NONE', #13754, #16239, #16422 ) ;
#10906 = EDGE_LOOP ( 'NONE', ( #12424, #8633, #6551, #16134 ) ) ;
#10907 = LINE ( 'NONE', #12165, #4226 ) ;
#10908 = CARTESIAN_POINT ( 'NONE',  ( 30.00000000000000355, 196.6227766016838245, -13.00000000000000000 ) ) ;
#10909 = CARTESIAN_POINT ( 'NONE',  ( -15.77503540472913457, 32.61497647743762229, -7.787339510197840653 ) ) ;
#10910 = ORIENTED_EDGE ( 'NONE', *, *, #1384, .F. ) ;
#10911 = ORIENTED_EDGE ( 'NONE', *, *, #7545, .F. ) ;
#10912 = CARTESIAN_POINT ( 'NONE',  ( -27.99999999999998224, 10.00000000000000000, 0.000000000000000000 ) ) ;
#10913 = CARTESIAN_POINT ( 'NONE',  ( 12.26645298401004425, 138.5600601684519120, 12.85897773338031946 ) ) ;
#10914 = CIRCLE ( 'NONE', #17137, 2.500000000000002220 ) ;
#10915 = VECTOR ( 'NONE', #14348, 1000.000000000000000 ) ;
#10916 = ORIENTED_EDGE ( 'NONE', *, *, #3787, .T. ) ;
#10917 = CARTESIAN_POINT ( 'NONE',  ( -27.99999999999998224, 10.00000000000000000, -18.75000000000000355 ) ) ;
#10918 = FACE_OUTER_BOUND ( 'NONE', #7469, .T. ) ;
#10919 = AXIS2_PLACEMENT_3D ( 'NONE', #16130, #9385, #5224 ) ;
#10920 = EDGE_CURVE ( 'NONE', #588, #8971, #15342, .T. ) ;
#10921 = FACE_OUTER_BOUND ( 'NONE', #10224, .T. ) ;
#10922 = CARTESIAN_POINT ( 'NONE',  ( 15.98317902225257470, 29.97876603371781457, -12.94822346880645902 ) ) ;
#10923 = DIRECTION ( 'NONE',  ( 0.000000000000000000, 0.000000000000000000, 1.000000000000000000 ) ) ;
#10924 = CARTESIAN_POINT ( 'NONE',  ( -76.03376373747714467, 149.6716700844112040, 24.64096846353360704 ) ) ;
#10925 = ORIENTED_EDGE ( 'NONE', *, *, #7864, .T. ) ;
#10926 = CARTESIAN_POINT ( 'NONE',  ( -78.68705929748917072, 202.4787130041031560, -16.52010876963831620 ) ) ;
#10927 = CARTESIAN_POINT ( 'NONE',  ( 14.80502546477524817, 129.0472650296936479, 11.28997929065621797 ) ) ;
#10928 = CARTESIAN_POINT ( 'NONE',  ( 34.93420767853314146, 20.00000000000000000, -6.320602137672510779 ) ) ;
#10929 = DIRECTION ( 'NONE',  ( -1.000000000000000000, -0.000000000000000000, -0.000000000000000000 ) ) ;
#10930 = DIRECTION ( 'NONE',  ( -1.000000000000000000, -0.000000000000000000, -0.000000000000000000 ) ) ;
#10931 = AXIS2_PLACEMENT_3D ( 'NONE', #1686, #1590, #5835 ) ;
#10932 = EDGE_LOOP ( 'NONE', ( #4106, #12016, #10535, #7244 ) ) ;
#10933 = VECTOR ( 'NONE', #10169, 1000.000000000000000 ) ;
#10934 =( GEOMETRIC_REPRESENTATION_CONTEXT ( 3 ) GLOBAL_UNCERTAINTY_ASSIGNED_CONTEXT ( ( #16919 ) ) GLOBAL_UNIT_ASSIGNED_CONTEXT ( ( #12805, #8553, #15286 ) ) REPRESENTATION_CONTEXT ( 'NONE', 'WORKASPACE' ) );
#10935 = VECTOR ( 'NONE', #5111, 1000.000000000000000 ) ;
#10936 = CARTESIAN_POINT ( 'NONE',  ( 35.00000000000000000, 196.6227766016838245, -12.99999999999999822 ) ) ;
#10937 =( REPRESENTATION_RELATIONSHIP ('NONE','NONE', #9723, #12790 ) REPRESENTATION_RELATIONSHIP_WITH_TRANSFORMATION ( #12782 )SHAPE_REPRESENTATION_RELATIONSHIP( ) );
#10938 = ORIENTED_EDGE ( 'NONE', *, *, #9874, .T. ) ;
#10939 = CARTESIAN_POINT ( 'NONE',  ( -32.93725393319379435, 120.0000000000000284, 5.500000000000000000 ) ) ;
#10940 = ORIENTED_EDGE ( 'NONE', *, *, #11708, .T. ) ;
#10941 = LINE ( 'NONE', #239, #12453 ) ;
#10942 = EDGE_CURVE ( 'NONE', #4284, #5792, #3534, .T. ) ;
#10943 = AXIS2_PLACEMENT_3D ( 'NONE', #7688, #7604, #6359 ) ;
#10944 = PLANE ( 'NONE',  #5804 ) ;
#10945 = CARTESIAN_POINT ( 'NONE',  ( -207.4300157105867015, 166.4745706146902364, 0.9272066051987427615 ) ) ;
#10946 = AXIS2_PLACEMENT_3D ( 'NONE', #6444, #4937, #9094 ) ;
#10947 = DIRECTION ( 'NONE',  ( -1.000000000000000000, 0.000000000000000000, 0.000000000000000000 ) ) ;
#10948 = CIRCLE ( 'NONE', #1635, 2.500000000000000000 ) ;
#10949 = ORIENTED_EDGE ( 'NONE', *, *, #10632, .F. ) ;
#10950 = DIRECTION ( 'NONE',  ( 0.000000000000000000, -1.000000000000000000, 0.000000000000000000 ) ) ;
#10951 = EDGE_CURVE ( 'NONE', #1170, #17378, #136, .T. ) ;
#10952 = CARTESIAN_POINT ( 'NONE',  ( -43.00000000000000000, 171.6227766016838245, 0.000000000000000000 ) ) ;
#10953 = DIRECTION ( 'NONE',  ( 0.000000000000000000, 1.040834085586084059E-15, 1.000000000000000000 ) ) ;
#10954 = EDGE_CURVE ( 'NONE', #5946, #15177, #4663, .T. ) ;
#10955 = ADVANCED_FACE ( 'NONE', ( #9118 ), #3468, .F. ) ;
#10956 = PRODUCT_DEFINITION_SHAPE ( 'NONE', 'NONE',  #17530 ) ;
#10957 = CARTESIAN_POINT ( 'NONE',  ( 18.85693063296981009, 140.6075696125688239, -16.22282984566914621 ) ) ;
#10958 = AXIS2_PLACEMENT_3D ( 'NONE', #15614, #3489, #11626 ) ;
#10959 = ORIENTED_EDGE ( 'NONE', *, *, #6191, .T. ) ;
#10960 = CARTESIAN_POINT ( 'NONE',  ( 48.00000000000000711, 151.6227766016839098, 3.071800142134974099 ) ) ;
#10961 = CIRCLE ( 'NONE', #7004, 747.9999999999998863 ) ;
#10962 = LINE ( 'NONE', #4245, #6372 ) ;
#10963 = VERTEX_POINT ( 'NONE', #15858 ) ;
#10964 = CARTESIAN_POINT ( 'NONE',  ( -32.65377812985267525, 119.1901795341236578, -4.906772863005508079 ) ) ;
#10965 = B_SPLINE_CURVE_WITH_KNOTS ( 'NONE', 3,
 ( #13154, #7665, #2180, #15718, #8991, #3870, #14402, #3512, #7745, #2270, #15813, #11912, #12001, #5276, #10579, #15988, #4920, #14664, #10496, #5012, #942, #17405, #7839, #11724, #7935 ),
 .UNSPECIFIED., .F., .F.,
 ( 4, 2, 2, 2, 2, 2, 2, 2, 2, 1, 2, 2, 4 ),
 ( 0.000000000000000000, 0.001953037758357041142, 0.002929556637535561930, 0.003906075516714082284, 0.005859113275071132533, 0.006835632154249659392, 0.007812151033428187119, 0.009765188791785242572, 0.01074170767096376509, 0.01171822655014228762, 0.01269474542932080841, 0.01367126430849933093, 0.01562430206685638465 ),
 .UNSPECIFIED. ) ;
#10966 = CARTESIAN_POINT ( 'NONE',  ( 1.559999999999998943, 0.000000000000000000, 0.000000000000000000 ) ) ;
#10967 = DIRECTION ( 'NONE',  ( 0.000000000000000000, -1.000000000000000000, 0.000000000000000000 ) ) ;
#10968 = CARTESIAN_POINT ( 'NONE',  ( 34.80468147095351128, 17.99999999999999645, -7.619145204522578041 ) ) ;
#10969 = LINE ( 'NONE', #16393, #11504 ) ;
#10970 = CARTESIAN_POINT ( 'NONE',  ( 22.12508471281541134, 29.85770821936580433, 8.546410110412809402 ) ) ;
#10971 = VECTOR ( 'NONE', #12355, 1000.000000000000000 ) ;
#10972 = CARTESIAN_POINT ( 'NONE',  ( 49.99999999999998579, 191.6227766016837677, -3.071800142134975431 ) ) ;
#10973 = AXIS2_PLACEMENT_3D ( 'NONE', #5832, #13714, #9902 ) ;
#10974 = LINE ( 'NONE', #7600, #14564 ) ;
#10975 = ORIENTED_EDGE ( 'NONE', *, *, #11916, .T. ) ;
#10976 = CARTESIAN_POINT ( 'NONE',  ( -19.80886414215398261, 19.99999999999999645, -20.97268729564270728 ) ) ;
#10977 = VERTEX_POINT ( 'NONE', #816 ) ;
#10978 = DIRECTION ( 'NONE',  ( -1.000000000000000000, -0.000000000000000000, 0.000000000000000000 ) ) ;
#10979 = CARTESIAN_POINT ( 'NONE',  ( 36.00000000000000711, 196.6227766016838245, -24.49489742783179125 ) ) ;
#10980 = ORIENTED_EDGE ( 'NONE', *, *, #5830, .T. ) ;
#10981 = CARTESIAN_POINT ( 'NONE',  ( -27.98221281341758626, 19.99999999999999645, 6.321711414556861364 ) ) ;
#10982 = CARTESIAN_POINT ( 'NONE',  ( -85.00000000000002842, 146.6227766016838245, -35.00200000000000244 ) ) ;
#10983 = EDGE_CURVE ( 'NONE', #793, #9467, #10450, .T. ) ;
#10984 = ORIENTED_EDGE ( 'NONE', *, *, #16290, .T. ) ;
#10985 = EDGE_CURVE ( 'NONE', #14433, #9729, #14190, .T. ) ;
#10986 = AXIS2_PLACEMENT_3D ( 'NONE', #3771, #14832, #5458 ) ;
#10987 = DIRECTION ( 'NONE',  ( -1.000000000000000000, 0.000000000000000000, 0.000000000000000000 ) ) ;
#10988 = AXIS2_PLACEMENT_3D ( 'NONE', #8835, #7590, #7246 ) ;
#10989 = ORIENTED_EDGE ( 'NONE', *, *, #1766, .F. ) ;
#10990 = CARTESIAN_POINT ( 'NONE',  ( -95.00000000000000000, 201.6227766016838245, 1.836970198721029589E-15 ) ) ;
#10991 = CARTESIAN_POINT ( 'NONE',  ( 15.60228996708978855, 124.9392590763941371, 1.387778780781445676E-14 ) ) ;
#10992 = CARTESIAN_POINT ( 'NONE',  ( 6.134011831684053284, 134.2062027339443944, 15.00000000000000000 ) ) ;
#10993 = EDGE_LOOP ( 'NONE', ( #15714, #16613, #15363, #8632 ) ) ;
#10994 = CARTESIAN_POINT ( 'NONE',  ( -40.00000000000000711, 8.000000000000000000, 30.00000000000000711 ) ) ;
#10995 = VERTEX_POINT ( 'NONE', #15507 ) ;
#10996 = CARTESIAN_POINT ( 'NONE',  ( 23.67803828928656884, 138.9414820825090544, -12.55787835418278675 ) ) ;
#10997 = AXIS2_PLACEMENT_3D ( 'NONE', #8543, #9869, #9954 ) ;
#10998 = ORIENTED_EDGE ( 'NONE', *, *, #320, .T. ) ;
#10999 = CARTESIAN_POINT ( 'NONE',  ( -86.34904889156064201, 192.6231533511310374, -25.45681811525071225 ) ) ;
#11000 = AXIS2_PLACEMENT_3D ( 'NONE', #2172, #7569, #857 ) ;
#11001 = CARTESIAN_POINT ( 'NONE',  ( -40.00000000000000000, 20.00000000000000000, 28.00000000000000355 ) ) ;
#11002 = DIRECTION ( 'NONE',  ( 1.000000000000000000, 0.000000000000000000, -0.000000000000000000 ) ) ;
#11003 = VERTEX_POINT ( 'NONE', #13108 ) ;
#11004 = ORIENTED_EDGE ( 'NONE', *, *, #2354, .T. ) ;
#11005 = CARTESIAN_POINT ( 'NONE',  ( -16.30611068361787019, 32.76923076923078781, 0.000000000000000000 ) ) ;
#11006 = ADVANCED_FACE ( 'NONE', ( #6210 ), #8855, .F. ) ;
#11007 = EDGE_CURVE ( 'NONE', #7044, #6861, #11608, .T. ) ;
#11008 = CARTESIAN_POINT ( 'NONE',  ( 196.0000000000000000, 171.6227766016838245, 12.50000337241049131 ) ) ;
#11009 = EDGE_CURVE ( 'NONE', #10138, #10436, #6915, .T. ) ;
#11010 = CARTESIAN_POINT ( 'NONE',  ( 10.91733900447607830, 142.2434614804602404, 19.02291218241819593 ) ) ;
#11011 = AXIS2_PLACEMENT_3D ( 'NONE', #1046, #5395, #1222 ) ;
#11012 = EDGE_LOOP ( 'NONE', ( #7567, #11210, #8322, #15947 ) ) ;
#11013 = APPLICATION_PROTOCOL_DEFINITION ( 'draft international standard', 'automotive_design', 1998, #7328 ) ;
#11014 = DIRECTION ( 'NONE',  ( 1.000000000000000000, -0.000000000000000000, -0.000000000000000000 ) ) ;
#11015 = VECTOR ( 'NONE', #12057, 1000.000000000000000 ) ;
#11016 = DIRECTION ( 'NONE',  ( 0.000000000000000000, -0.000000000000000000, -1.000000000000000000 ) ) ;
#11017 = DIRECTION ( 'NONE',  ( -1.000000000000000000, -0.000000000000000000, -0.000000000000000000 ) ) ;
#11018 = DIRECTION ( 'NONE',  ( 1.000000000000000000, 0.000000000000000000, 0.000000000000000000 ) ) ;
#11019 = CARTESIAN_POINT ( 'NONE',  ( 23.18512258076444610, 18.00000000000000000, 23.22991426836919615 ) ) ;
#11020 = EDGE_LOOP ( 'NONE', ( #4016, #5620 ) ) ;
#11021 = DIRECTION ( 'NONE',  ( 1.000000000000000000, 0.000000000000000000, 0.000000000000000000 ) ) ;
#11022 = DIRECTION ( 'NONE',  ( 0.000000000000000000, 0.000000000000000000, -1.000000000000000000 ) ) ;
#11023 = CARTESIAN_POINT ( 'NONE',  ( -24.94987437106622252, 100.0000000000000142, -6.000000000000000000 ) ) ;
#11024 = CARTESIAN_POINT ( 'NONE',  ( -45.00000000000000000, 122.0000000000000142, -15.00000000000000000 ) ) ;
#11025 = DIRECTION ( 'NONE',  ( 0.000000000000000000, -1.000000000000000000, 0.000000000000000000 ) ) ;
#11026 = PRODUCT_DEFINITION_CONTEXT ( 'detailed design', #14555, 'design' ) ;
#11027 = CIRCLE ( 'NONE', #12171, 2.500000000000002220 ) ;
#11028 = AXIS2_PLACEMENT_3D ( 'NONE', #6813, #16008, #12019 ) ;
#11029 = ORIENTED_EDGE ( 'NONE', *, *, #1318, .T. ) ;
#11030 = EDGE_CURVE ( 'NONE', #13521, #4808, #7531, .T. ) ;
#11031 = VECTOR ( 'NONE', #8910, 1000.000000000000000 ) ;
#11032 = CARTESIAN_POINT ( 'NONE',  ( -197.9999999999999716, 171.6227766016838245, 8.000000000000007105 ) ) ;
#11033 = VERTEX_POINT ( 'NONE', #17013 ) ;
#11034 = VERTEX_POINT ( 'NONE', #14521 ) ;
#11035 = CARTESIAN_POINT ( 'NONE',  ( -84.59125389484567847, 144.6221806392915425, 18.97834816100454702 ) ) ;
#11036 = DIRECTION ( 'NONE',  ( 0.000000000000000000, -1.000000000000000000, 0.000000000000000000 ) ) ;
#11037 = CARTESIAN_POINT ( 'NONE',  ( -77.50000000000001421, 196.6227766016838245, -16.00000000000000000 ) ) ;
#11038 = AXIS2_PLACEMENT_3D ( 'NONE', #9624, #14685, #2902 ) ;
#11039 = AXIS2_PLACEMENT_3D ( 'NONE', #15096, #16188, #2811 ) ;
#11040 = ORIENTED_EDGE ( 'NONE', *, *, #7387, .F. ) ;
#11041 = DIRECTION ( 'NONE',  ( -1.000000000000000000, -0.000000000000000000, 0.000000000000000000 ) ) ;
#11042 = CARTESIAN_POINT ( 'NONE',  ( 48.00000000000000711, 191.6227766016837677, -8.071800142134975431 ) ) ;
#11043 = DIRECTION ( 'NONE',  ( 1.000000000000000000, 0.000000000000000000, 0.000000000000000000 ) ) ;
#11044 =( NAMED_UNIT ( * ) SI_UNIT ( $, .STERADIAN. ) SOLID_ANGLE_UNIT ( ) );
#11045 =( REPRESENTATION_RELATIONSHIP ('NONE','NONE', #9723, #10772 ) REPRESENTATION_RELATIONSHIP_WITH_TRANSFORMATION ( #3310 )SHAPE_REPRESENTATION_RELATIONSHIP( ) );
#11046 = EDGE_CURVE ( 'NONE', #11034, #11927, #9742, .T. ) ;
#11047 = VECTOR ( 'NONE', #9420, 1000.000000000000000 ) ;
#11048 = CARTESIAN_POINT ( 'NONE',  ( 17.52204077229825785, 125.6458339596819798, -5.684362142990314837 ) ) ;
#11049 = VERTEX_POINT ( 'NONE', #3732 ) ;
#11050 = DIRECTION ( 'NONE',  ( 0.000000000000000000, 0.000000000000000000, -1.000000000000000000 ) ) ;
#11051 = CARTESIAN_POINT ( 'NONE',  ( 15.26338903195270547, 125.9505563168691111, -6.751637631526196337 ) ) ;
#11052 = ORIENTED_EDGE ( 'NONE', *, *, #1955, .T. ) ;
#11053 = CARTESIAN_POINT ( 'NONE',  ( -82.40832088953489176, 191.1229741556853128, -29.06467671913510031 ) ) ;
#11054 = EDGE_CURVE ( 'NONE', #11464, #16539, #11954, .T. ) ;
#11055 = ADVANCED_FACE ( 'NONE', ( #12222 ), #13465, .F. ) ;
#11056 = FACE_OUTER_BOUND ( 'NONE', #7678, .T. ) ;
#11057 = DIRECTION ( 'NONE',  ( 0.000000000000000000, -0.5000000000000011102, -0.8660254037844379305 ) ) ;
#11058 = CARTESIAN_POINT ( 'NONE',  ( -15.00000000000002665, 130.0000000000000000, -15.00000000000000000 ) ) ;
#11059 = DIRECTION ( 'NONE',  ( -1.000000000000000000, 0.000000000000000000, 5.782411586589356653E-16 ) ) ;
#11060 = CIRCLE ( 'NONE', #325, 2.500000000000002220 ) ;
#11061 = CARTESIAN_POINT ( 'NONE',  ( 20.22365234301270931, 29.89465715177047400, 11.02453202869212312 ) ) ;
#11062 = CARTESIAN_POINT ( 'NONE',  ( -197.9999999999999716, 171.6227766016838245, -8.000000000000007105 ) ) ;
#11063 = FILL_AREA_STYLE ('',( #3271 ) ) ;
#11064 = ORIENTED_EDGE ( 'NONE', *, *, #5964, .T. ) ;
#11065 = ORIENTED_EDGE ( 'NONE', *, *, #7151, .F. ) ;
#11066 = FACE_OUTER_BOUND ( 'NONE', #8539, .T. ) ;
#11067 = DIRECTION ( 'NONE',  ( -1.000000000000000000, -0.000000000000000000, -0.000000000000000000 ) ) ;
#11068 = VERTEX_POINT ( 'NONE', #13557 ) ;
#11069 = PLANE ( 'NONE',  #1260 ) ;
#11070 = CYLINDRICAL_SURFACE ( 'NONE', #2191, 25.69059892324149175 ) ;
#11071 = ORIENTED_EDGE ( 'NONE', *, *, #16534, .T. ) ;
#11072 = CARTESIAN_POINT ( 'NONE',  ( -33.00000000000000711, 171.6227766016838245, 0.000000000000000000 ) ) ;
#11073 = EDGE_CURVE ( 'NONE', #3234, #2441, #17356, .T. ) ;
#11074 =( BOUNDED_SURFACE ( )  B_SPLINE_SURFACE ( 3, 2, ( 
 ( #5132, #9018, #11847 ),
 ( #6547, #10519, #14688 ),
 ( #3794, #962, #9281 ),
 ( #2471, #2571, #1228 ),
 ( #17340, #10701, #13017 ),
 ( #7958, #16117, #7769 ),
 ( #3990, #890, #6278 ),
 ( #11668, #17077, #4946 ),
 ( #7863, #10341, #17255 ),
 ( #3628, #2296, #11754 ),
 ( #17165, #13277, #5038 ),
 ( #10431, #15844, #9103 ),
 ( #13447, #253, #10957 ),
 ( #16463, #1412, #1495 ),
 ( #2988, #8038, #159 ),
 ( #6816, #16281, #13538 ),
 ( #4153, #10864, #2905 ),
 ( #9712, #12470, #2648 ),
 ( #1317, #4326, #13704 ),
 ( #6886, #11126, #12209 ),
 ( #4242, #6724, #338 ),
 ( #9446, #5477, #8217 ),
 ( #1579, #12123, #5740 ),
 ( #13806, #5565, #6978 ),
 ( #16544, #16376, #4068 ),
 ( #14856, #9374, #14776 ),
 ( #12285, #7563, #9627 ),
 ( #15027, #5399, #8389 ),
 ( #11048, #8294, #1674 ),
 ( #12377, #75, #7072 ) ),
 .UNSPECIFIED., .F., .F., .F. ) 
 B_SPLINE_SURFACE_WITH_KNOTS ( ( 4, 2, 2, 2, 2, 2, 2, 2, 2, 2, 2, 2, 2, 2, 4 ),
 ( 3, 3 ),
 ( 0.01165250788892074896, 0.01579789672993320987, 0.01787059115043944033, 0.01890693836069255729, 0.01994328557094567078, 0.02408867441195813169, 0.02616136883246436215, 0.02823406325297059261, 0.03030675767347682306, 0.03237945209398305352, 0.03652484093499551443, 0.03859753535550174142, 0.03963388256575485491, 0.04067022977600797534, 0.04481561861702043625 ),
 ( 0.000000000000000000, 1.000000000000000000 ),
 .UNSPECIFIED. ) 
 GEOMETRIC_REPRESENTATION_ITEM ( )  RATIONAL_B_SPLINE_SURFACE ( (
 ( 1.000000000000000000, 0.8819171036881967574, 1.000000000000000000),
 ( 1.000000000000000000, 0.8793942645247267986, 1.000000000000000000),
 ( 1.000000000000000000, 0.8749458316895478704, 1.000000000000000000),
 ( 1.000000000000000000, 0.8656814021268812720, 1.000000000000000000),
 ( 1.000000000000000000, 0.8621600075896179716, 1.000000000000000000),
 ( 1.000000000000000000, 0.8562492930711324002, 1.000000000000000000),
 ( 1.000000000000000000, 0.8541736901085718037, 1.000000000000000000),
 ( 1.000000000000000000, 0.8498659178639272893, 1.000000000000000000),
 ( 1.000000000000000000, 0.8476283308601378907, 1.000000000000000000),
 ( 1.000000000000000000, 0.8360458749412158497, 1.000000000000000000),
 ( 1.000000000000000000, 0.8255221978280062878, 1.000000000000000000),
 ( 1.000000000000000000, 0.8082270345002190437, 1.000000000000000000),
 ( 1.000000000000000000, 0.8022128341710524913, 1.000000000000000000),
 ( 1.000000000000000000, 0.7899684886178014454, 1.000000000000000000),
 ( 1.000000000000000000, 0.7837128169315926707, 1.000000000000000000),
 ( 1.000000000000000000, 0.7710263478624882483, 1.000000000000000000),
 ( 1.000000000000000000, 0.7645952338536526893, 1.000000000000000000),
 ( 1.000000000000000000, 0.7516613202048504361, 1.000000000000000000),
 ( 1.000000000000000000, 0.7451386183437513910, 1.000000000000000000),
 ( 1.000000000000000000, 0.7257808243684673588, 1.000000000000000000),
 ( 1.000000000000000000, 0.7133953845776390690, 1.000000000000000000),
 ( 1.000000000000000000, 0.6965170042221164870, 1.000000000000000000),
 ( 1.000000000000000000, 0.6911767420095684678, 1.000000000000000000),
 ( 1.000000000000000000, 0.6837405640632492343, 1.000000000000000000),
 ( 1.000000000000000000, 0.6813577907325653049, 1.000000000000000000),
 ( 1.000000000000000000, 0.6768117804539316440, 1.000000000000000000),
 ( 1.000000000000000000, 0.6746439590912862716, 1.000000000000000000),
 ( 1.000000000000000000, 0.6645663254999056857, 1.000000000000000000),
 ( 1.000000000000000000, 0.6588263891901358082, 1.000000000000000000),
 ( 1.000000000000000000, 0.6558243695371221982, 1.000000000000000000) ) ) 
 REPRESENTATION_ITEM ( '' )  SURFACE ( )  );
#11075 = CARTESIAN_POINT ( 'NONE',  ( -24.99999999999999289, 90.00000000000000000, 0.000000000000000000 ) ) ;
#11076 = DIRECTION ( 'NONE',  ( -0.000000000000000000, -0.000000000000000000, -1.000000000000000000 ) ) ;
#11077 = CARTESIAN_POINT ( 'NONE',  ( 37.25061104762458797, 194.6575378623844585, -23.63707964515041482 ) ) ;
#11078 = CARTESIAN_POINT ( 'NONE',  ( -34.99999999999999289, 120.0000000000000284, -4.999999999999999112 ) ) ;
#11079 = CARTESIAN_POINT ( 'NONE',  ( -68.00000000000000000, 171.6227766016838245, -2.296212748401287183E-15 ) ) ;
#11080 = CARTESIAN_POINT ( 'NONE',  ( -73.00000000000001421, 171.6227766016838245, 19.49999999999998934 ) ) ;
#11081 = ORIENTED_EDGE ( 'NONE', *, *, #14694, .F. ) ;
#11082 = DIRECTION ( 'NONE',  ( 1.000000000000000000, 0.000000000000000000, 0.000000000000000000 ) ) ;
#11083 = EDGE_CURVE ( 'NONE', #9695, #16992, #2693, .T. ) ;
#11084 = ORIENTED_EDGE ( 'NONE', *, *, #16793, .F. ) ;
#11085 = DIRECTION ( 'NONE',  ( -1.000000000000000000, 0.000000000000000000, 0.000000000000000000 ) ) ;
#11086 = CARTESIAN_POINT ( 'NONE',  ( -100.0000000000000000, 120.0000000000000284, -6.000000000000001776 ) ) ;
#11087 = CARTESIAN_POINT ( 'NONE',  ( -32.66708739526901439, 118.9256703196821263, -4.648821459087186803 ) ) ;
#11088 = ORIENTED_EDGE ( 'NONE', *, *, #5752, .T. ) ;
#11089 = ORIENTED_EDGE ( 'NONE', *, *, #9112, .T. ) ;
#11090 = DIRECTION ( 'NONE',  ( -1.000000000000000000, -0.000000000000000000, -0.000000000000000000 ) ) ;
#11091 = CARTESIAN_POINT ( 'NONE',  ( 15.96677753504215858, 136.6227766016837961, 4.434194661153730915E-13 ) ) ;
#11092 = CARTESIAN_POINT ( 'NONE',  ( 16.01769397135268491, 136.8393535285714506, 3.937079669079953437 ) ) ;
#11093 = ORIENTED_EDGE ( 'NONE', *, *, #2820, .T. ) ;
#11094 =( NAMED_UNIT ( * ) PLANE_ANGLE_UNIT ( ) SI_UNIT ( $, .RADIAN. ) );
#11095 = CARTESIAN_POINT ( 'NONE',  ( -95.00000000000000000, 199.3133755249253056, 0.000000000000000000 ) ) ;
#11096 = MANIFOLD_SOLID_BREP ( 'Fillet1', #12049 ) ;
#11097 = CYLINDRICAL_SURFACE ( 'NONE', #10631, 5.000000000000004441 ) ;
#11098 = DIRECTION ( 'NONE',  ( 1.000000000000000000, 0.000000000000000000, 0.000000000000000000 ) ) ;
#11099 = CARTESIAN_POINT ( 'NONE',  ( -40.00000000000000000, 20.00000000000000000, 0.000000000000000000 ) ) ;
#11100 = CARTESIAN_POINT ( 'NONE',  ( 17.56962100350864375, 125.3109322897003608, 3.333333333333324600 ) ) ;
#11101 = ORIENTED_EDGE ( 'NONE', *, *, #12702, .T. ) ;
#11102 = CARTESIAN_POINT ( 'NONE',  ( 30.00000000000001066, 146.6227766016838245, 10.00000000000000178 ) ) ;
#11103 = ADVANCED_FACE ( 'NONE', ( #10720 ), #5228, .F. ) ;
#11104 = ADVANCED_FACE ( 'NONE', ( #2587 ), #1163, .F. ) ;
#11105 = DIRECTION ( 'NONE',  ( 0.000000000000000000, 0.000000000000000000, -1.000000000000000000 ) ) ;
#11106 = EDGE_CURVE ( 'NONE', #4216, #1489, #9187, .T. ) ;
#11107 = CARTESIAN_POINT ( 'NONE',  ( 21.38845554303141938, 19.99999999999999289, -23.94082098111162082 ) ) ;
#11108 = FACE_OUTER_BOUND ( 'NONE', #10652, .T. ) ;
#11109 = PLANE ( 'NONE',  #2732 ) ;
#11110 = ADVANCED_FACE ( 'NONE', ( #11955 ), #14709, .F. ) ;
#11111 = ORIENTED_EDGE ( 'NONE', *, *, #2329, .F. ) ;
#11112 = VERTEX_POINT ( 'NONE', #9820 ) ;
#11113 = DIRECTION ( 'NONE',  ( -1.000000000000000000, 0.000000000000000000, 0.000000000000000000 ) ) ;
#11114 = VERTEX_POINT ( 'NONE', #5753 ) ;
#11115 = PLANE ( 'NONE',  #200 ) ;
#11116 = EDGE_LOOP ( 'NONE', ( #8830, #13428, #8626, #1050 ) ) ;
#11117 = PLANE ( 'NONE',  #13310 ) ;
#11118 = PLANE ( 'NONE',  #2986 ) ;
#11119 = LINE ( 'NONE', #7060, #8439 ) ;
#11120 = CYLINDRICAL_SURFACE ( 'NONE', #12876, 7.499999999999996447 ) ;
#11121 = ORIENTED_EDGE ( 'NONE', *, *, #1030, .T. ) ;
#11122 = CARTESIAN_POINT ( 'NONE',  ( 32.94787740378740892, 142.5723011982436788, 15.66001370690270633 ) ) ;
#11123 = LINE ( 'NONE', #154, #16109 ) ;
#11124 = CARTESIAN_POINT ( 'NONE',  ( -22.99999999999999645, 90.00000000000000000, 0.000000000000000000 ) ) ;
#11125 = DIRECTION ( 'NONE',  ( 0.000000000000000000, 0.000000000000000000, 1.000000000000000000 ) ) ;
#11126 = CARTESIAN_POINT ( 'NONE',  ( 16.25737266305939599, 136.9911583880083015, -7.117438641154834045 ) ) ;
#11127 = EDGE_LOOP ( 'NONE', ( #976, #4793, #13727, #6048 ) ) ;
#11128 = CARTESIAN_POINT ( 'NONE',  ( -208.0000000000000853, 170.0678595944000620, 2.693195258168412654 ) ) ;
#11129 = EDGE_LOOP ( 'NONE', ( #1740, #11845 ) ) ;
#11130 = SHAPE_REPRESENTATION_RELATIONSHIP ( 'NONE' , 'NONE' ,  #16423, #5730 ) ;
#11131 = CARTESIAN_POINT ( 'NONE',  ( -85.03936963251346981, 193.3606217133605583, -27.43184792633612545 ) ) ;
#11132 = DIRECTION ( 'NONE',  ( 1.000000000000000000, 0.000000000000000000, 0.000000000000000000 ) ) ;
#11133 = CARTESIAN_POINT ( 'NONE',  ( 29.22485437292392518, 191.6792914357319546, 26.20566807848922153 ) ) ;
#11134 = EDGE_CURVE ( 'NONE', #9063, #15728, #7765, .T. ) ;
#11135 = CARTESIAN_POINT ( 'NONE',  ( 49.99999999999998579, 179.6227766016838245, -12.50000337241049309 ) ) ;
#11136 = LINE ( 'NONE', #15121, #4727 ) ;
#11137 = CARTESIAN_POINT ( 'NONE',  ( -43.00000000000001421, 125.3137084989847665, 13.00000000000000178 ) ) ;
#11138 = CARTESIAN_POINT ( 'NONE',  ( -82.08787771659024202, 201.1698135001049934, 14.69689982759750535 ) ) ;
#11139 = FACE_BOUND ( 'NONE', #14973, .T. ) ;
#11140 = CIRCLE ( 'NONE', #8321, 24.99999999999999645 ) ;
#11141 = ORIENTED_EDGE ( 'NONE', *, *, #7953, .T. ) ;
#11142 = CIRCLE ( 'NONE', #3522, 25.69059892324149175 ) ;
#11143 = VERTEX_POINT ( 'NONE', #268 ) ;
#11144 = CARTESIAN_POINT ( 'NONE',  ( -34.99999999999999289, 130.0000000000000000, 0.000000000000000000 ) ) ;
#11145 = DIRECTION ( 'NONE',  ( 0.000000000000000000, 0.000000000000000000, -1.000000000000000000 ) ) ;
#11146 = ORIENTED_EDGE ( 'NONE', *, *, #11588, .T. ) ;
#11147 = LINE ( 'NONE', #16566, #5780 ) ;
#11148 = MANIFOLD_SOLID_BREP ( 'Boss-Extrude4', #6380 ) ;
#11149 = DIRECTION ( 'NONE',  ( 1.000000000000000000, -0.000000000000000000, -0.000000000000000000 ) ) ;
#11150 = ORIENTED_EDGE ( 'NONE', *, *, #8256, .F. ) ;
#11151 = CARTESIAN_POINT ( 'NONE',  ( 35.45105639388463459, 151.7804781109684313, -26.36917907415268658 ) ) ;
#11152 = CIRCLE ( 'NONE', #8621, 20.00000000000000355 ) ;
#11153 = DIRECTION ( 'NONE',  ( 0.000000000000000000, 0.000000000000000000, 1.000000000000000000 ) ) ;
#11154 = CIRCLE ( 'NONE', #4388, 2.500000000000002220 ) ;
#11155 = ADVANCED_FACE ( 'NONE', ( #13826 ), #13724, .T. ) ;
#11156 = DIRECTION ( 'NONE',  ( 0.000000000000000000, 0.000000000000000000, 1.000000000000000000 ) ) ;
#11157 = CARTESIAN_POINT ( 'NONE',  ( 27.75000000000000000, 0.000000000000000000, 0.000000000000000000 ) ) ;
#11158 = CARTESIAN_POINT ( 'NONE',  ( -3.000000000000000888, 191.6227766016837961, -1.224646799147353454E-15 ) ) ;
#11159 = CARTESIAN_POINT ( 'NONE',  ( 1.559999999999998943, -0.8660254037844428154, 1.500000000000001332 ) ) ;
#11160 = FACE_OUTER_BOUND ( 'NONE', #12587, .T. ) ;
#11161 = VERTEX_POINT ( 'NONE', #15041 ) ;
#11162 = LINE ( 'NONE', #3206, #810 ) ;
#11163 = EDGE_CURVE ( 'NONE', #9872, #6476, #1839, .T. ) ;
#11164 =( REPRESENTATION_RELATIONSHIP ('NONE','NONE', #9723, #6585 ) REPRESENTATION_RELATIONSHIP_WITH_TRANSFORMATION ( #3403 )SHAPE_REPRESENTATION_RELATIONSHIP( ) );
#11165 = VERTEX_POINT ( 'NONE', #4433 ) ;
#11166 = ADVANCED_FACE ( 'NONE', ( #11139, #3101, #1594, #433, #8498, #13911, #1772, #7167, #2919, #16743, #4608, #15393, #12565, #11235 ), #8674, .F. ) ;
#11167 = CARTESIAN_POINT ( 'NONE',  ( -72.50701606102703067, 196.2445469595302825, -21.97388680505723713 ) ) ;
#11168 = ADVANCED_FACE ( 'NONE', ( #1946 ), #5581, .T. ) ;
#11169 = VECTOR ( 'NONE', #9768, 1000.000000000000000 ) ;
#11170 = ORIENTED_EDGE ( 'NONE', *, *, #10879, .T. ) ;
#11171 = VECTOR ( 'NONE', #177, 1000.000000000000000 ) ;
#11172 = ORIENTED_EDGE ( 'NONE', *, *, #9878, .T. ) ;
#11173 = EDGE_LOOP ( 'NONE', ( #16415, #1059, #354, #8785 ) ) ;
#11174 = DIRECTION ( 'NONE',  ( -0.000000000000000000, -0.000000000000000000, 1.000000000000000000 ) ) ;
#11175 = VECTOR ( 'NONE', #8556, 1000.000000000000000 ) ;
#11176 = CARTESIAN_POINT ( 'NONE',  ( 22.72753210816244618, 139.3086630800672765, 13.45249220522710232 ) ) ;
#11177 = ORIENTED_EDGE ( 'NONE', *, *, #10942, .T. ) ;
#11178 = CONTEXT_DEPENDENT_SHAPE_REPRESENTATION ( #12762, #224 ) ;
#11179 = EDGE_CURVE ( 'NONE', #15042, #4201, #7348, .T. ) ;
#11180 = FACE_OUTER_BOUND ( 'NONE', #17058, .T. ) ;
#11181 = MANIFOLD_SOLID_BREP ( 'Boss-Extrude4', #2727 ) ;
#11182 = CARTESIAN_POINT ( 'NONE',  ( -95.00000000000000000, 171.6227766016838245, 0.000000000000000000 ) ) ;
#11183 = VECTOR ( 'NONE', #8644, 1000.000000000000000 ) ;
#11184 = CARTESIAN_POINT ( 'NONE',  ( -77.42411652054217086, 192.3210352480456606, 25.70268529851927752 ) ) ;
#11185 = CARTESIAN_POINT ( 'NONE',  ( -138.7106781186547266, 171.6227766016838245, 24.99999999999999289 ) ) ;
#11186 = CARTESIAN_POINT ( 'NONE',  ( 17.14315908062561533, 17.99999999999943157, 12.73566125713464636 ) ) ;
#11187 = ORIENTED_EDGE ( 'NONE', *, *, #303, .T. ) ;
#11188 = CARTESIAN_POINT ( 'NONE',  ( -74.03485743176636902, 197.3601060891146233, -23.72478281133074063 ) ) ;
#11189 = DIRECTION ( 'NONE',  ( 0.000000000000000000, 0.5000000000000012212, 0.8660254037844380415 ) ) ;
#11190 = CARTESIAN_POINT ( 'NONE',  ( 28.15871609335591685, 19.99999999999999289, -20.05978710182010971 ) ) ;
#11191 = CARTESIAN_POINT ( 'NONE',  ( -34.99999999999999289, 130.0000000000000000, 15.00000000000000000 ) ) ;
#11192 = DIRECTION ( 'NONE',  ( 0.000000000000000000, 1.000000000000000000, -1.224646799147353207E-16 ) ) ;
#11193 = ORIENTED_EDGE ( 'NONE', *, *, #7378, .T. ) ;
#11194 = ORIENTED_EDGE ( 'NONE', *, *, #10016, .F. ) ;
#11195 = FACE_OUTER_BOUND ( 'NONE', #5515, .T. ) ;
#11196 = VECTOR ( 'NONE', #13875, 1000.000000000000000 ) ;
#11197 = ORIENTED_EDGE ( 'NONE', *, *, #9481, .F. ) ;
#11198 = DIRECTION ( 'NONE',  ( -0.000000000000000000, -0.000000000000000000, 1.000000000000000000 ) ) ;
#11199 = ORIENTED_EDGE ( 'NONE', *, *, #4306, .F. ) ;
#11200 = EDGE_CURVE ( 'NONE', #15042, #925, #10974, .T. ) ;
#11201 = EDGE_CURVE ( 'NONE', #10746, #7694, #7426, .T. ) ;
#11202 = LINE ( 'NONE', #16715, #5391 ) ;
#11203 = EDGE_CURVE ( 'NONE', #2935, #457, #356, .T. ) ;
#11204 = FILL_AREA_STYLE ('',( #5996 ) ) ;
#11205 = CARTESIAN_POINT ( 'NONE',  ( -207.1416055535977137, 166.5694718092265418, 0.7516812309923592839 ) ) ;
#11206 = DIRECTION ( 'NONE',  ( 1.000000000000000000, 0.000000000000000000, 0.000000000000000000 ) ) ;
#11207 = CARTESIAN_POINT ( 'NONE',  ( 18.23439605415255471, 29.93382634594462743, -12.29196570735054728 ) ) ;
#11208 = CIRCLE ( 'NONE', #13481, 2.500000000000000444 ) ;
#11209 = AXIS2_PLACEMENT_3D ( 'NONE', #14099, #9924, #16575 ) ;
#11210 = ORIENTED_EDGE ( 'NONE', *, *, #4147, .F. ) ;
#11211 = CARTESIAN_POINT ( 'NONE',  ( 30.23275679183038278, 141.6224873770942736, 13.74709594552941994 ) ) ;
#11212 = CARTESIAN_POINT ( 'NONE',  ( -45.00000000000000711, 171.6227766016838245, -19.49999999999998224 ) ) ;
#11213 = VECTOR ( 'NONE', #2262, 1000.000000000000000 ) ;
#11214 = CARTESIAN_POINT ( 'NONE',  ( -27.98221281347037959, 20.00000000000000000, 15.00000000000000000 ) ) ;
#11215 = COLOUR_RGB ( '', 0.08235294, 0.09019608, 0.10196078) ;
#11216 = MANIFOLD_SOLID_BREP ( 'Boss-Extrude6', #1868 ) ;
#11217 = SURFACE_STYLE_USAGE ( .BOTH. , #11311 ) ;
#11218 = AXIS2_PLACEMENT_3D ( 'NONE', #11507, #13019, #12664 ) ;
#11219 = PLANE ( 'NONE',  #2555 ) ;
#11220 = ORIENTED_EDGE ( 'NONE', *, *, #11264, .F. ) ;
#11221 = FACE_OUTER_BOUND ( 'NONE', #6315, .T. ) ;
#11222 = ORIENTED_EDGE ( 'NONE', *, *, #3935, .T. ) ;
#11223 = EDGE_CURVE ( 'NONE', #9797, #2837, #8624, .T. ) ;
#11224 = EDGE_CURVE ( 'NONE', #903, #16562, #3892, .T. ) ;
#11225 = VECTOR ( 'NONE', #7459, 1000.000000000000114 ) ;
#11226 = CARTESIAN_POINT ( 'NONE',  ( 196.0000000000000000, 175.6227766016838530, -19.42820660268601074 ) ) ;
#11227 = PRESENTATION_LAYER_ASSIGNMENT (  '', '', ( #9239 ) ) ;
#11228 = AXIS2_PLACEMENT_3D ( 'NONE', #8281, #16185, #4397 ) ;
#11229 = CARTESIAN_POINT ( 'NONE',  ( 27.48361012698968864, 136.6227766016838245, 0.000000000000000000 ) ) ;
#11230 = CARTESIAN_POINT ( 'NONE',  ( -82.50000000000001421, 196.6227766016838245, 10.00000000000000178 ) ) ;
#11231 = DIRECTION ( 'NONE',  ( -1.000000000000000000, 0.000000000000000000, 0.000000000000000000 ) ) ;
#11232 = CARTESIAN_POINT ( 'NONE',  ( -48.00000000000000000, 154.3022685259950038, 9.999999999999900524 ) ) ;
#11233 = CARTESIAN_POINT ( 'NONE',  ( 16.17028938446068764, 143.0439382767918346, 16.49999999999050360 ) ) ;
#11234 = CARTESIAN_POINT ( 'NONE',  ( -81.55989001854683806, 201.3777828775944556, 14.27084532960631158 ) ) ;
#11235 = FACE_OUTER_BOUND ( 'NONE', #8987, .T. ) ;
#11236 = EDGE_LOOP ( 'NONE', ( #1004, #8148 ) ) ;
#11237 = VECTOR ( 'NONE', #8741, 1000.000000000000000 ) ;
#11238 = ORIENTED_EDGE ( 'NONE', *, *, #7920, .T. ) ;
#11239 = FACE_OUTER_BOUND ( 'NONE', #1435, .T. ) ;
#11240 = VECTOR ( 'NONE', #5138, 1000.000000000000000 ) ;
#11241 = CARTESIAN_POINT ( 'NONE',  ( -95.00000000000000000, 171.6227766016838245, 0.000000000000000000 ) ) ;
#11242 = ORIENTED_EDGE ( 'NONE', *, *, #12573, .T. ) ;
#11243 = ADVANCED_FACE ( 'NONE', ( #7955 ), #6930, .T. ) ;
#11244 = CARTESIAN_POINT ( 'NONE',  ( -15.18548748502429468, 20.00000000000000000, 6.873064813191830602 ) ) ;
#11245 = FACE_OUTER_BOUND ( 'NONE', #10700, .T. ) ;
#11246 = ORIENTED_EDGE ( 'NONE', *, *, #8084, .T. ) ;
#11247 = CARTESIAN_POINT ( 'NONE',  ( 31.17267072074456991, 154.0361450035975110, -27.92332374485729218 ) ) ;
#11248 = VECTOR ( 'NONE', #5654, 1000.000000000000000 ) ;
#11249 = CARTESIAN_POINT ( 'NONE',  ( -23.65835920965563233, 18.00000000000000000, 17.33937328557891533 ) ) ;
#11250 = CIRCLE ( 'NONE', #9553, 12.00000000000000000 ) ;
#11251 = AXIS2_PLACEMENT_3D ( 'NONE', #14516, #17443, #2655 ) ;
#11252 = CARTESIAN_POINT ( 'NONE',  ( -206.6026792233874403, 166.6884423960484014, -0.5648693273743904397 ) ) ;
#11253 = FACE_OUTER_BOUND ( 'NONE', #4629, .T. ) ;
#11254 = DIRECTION ( 'NONE',  ( 1.000000000000000000, 0.000000000000000000, 0.000000000000000000 ) ) ;
#11255 = DIRECTION ( 'NONE',  ( -0.000000000000000000, -0.000000000000000000, 1.000000000000000000 ) ) ;
#11256 = DIRECTION ( 'NONE',  ( -1.000000000000000000, 0.000000000000000000, 0.000000000000000000 ) ) ;
#11257 = ORIENTED_EDGE ( 'NONE', *, *, #12303, .F. ) ;
#11258 = DIRECTION ( 'NONE',  ( 1.000000000000000000, 0.000000000000000000, 0.000000000000000000 ) ) ;
#11259 = ORIENTED_EDGE ( 'NONE', *, *, #10942, .F. ) ;
#11260 = FACE_OUTER_BOUND ( 'NONE', #3657, .T. ) ;
#11261 = PLANE ( 'NONE',  #12603 ) ;
#11262 = VECTOR ( 'NONE', #7534, 1000.000000000000114 ) ;
#11263 = VERTEX_POINT ( 'NONE', #9185 ) ;
#11264 = EDGE_CURVE ( 'NONE', #5481, #13477, #2646, .T. ) ;
#11265 = DIRECTION ( 'NONE',  ( 0.000000000000000000, 0.000000000000000000, -1.000000000000000000 ) ) ;
#11266 = AXIS2_PLACEMENT_3D ( 'NONE', #4601, #14416, #10071 ) ;
#11267 = FACE_OUTER_BOUND ( 'NONE', #12153, .T. ) ;
#11268 = CARTESIAN_POINT ( 'NONE',  ( 16.36928288456784131, 136.8619714623083610, 5.700917076122240523 ) ) ;
#11269 = EDGE_LOOP ( 'NONE', ( #7816, #15953, #4301 ) ) ;
#11270 = ITEM_DEFINED_TRANSFORMATION ( 'NONE', 'NONE', #13798,  #3583 ) ;
#11271 = DIRECTION ( 'NONE',  ( -1.000000000000000000, 0.000000000000000000, 0.000000000000000000 ) ) ;
#11272 = AXIS2_PLACEMENT_3D ( 'NONE', #8457, #13952, #317 ) ;
#11273 = ADVANCED_FACE ( 'NONE', ( #1225 ), #11844, .T. ) ;
#11274 = CARTESIAN_POINT ( 'NONE',  ( -74.00000000000002842, 146.6227766016838245, -35.00000000000000000 ) ) ;
#11275 = ADVANCED_FACE ( 'NONE', ( #10698, #4151 ), #6630, .T. ) ;
#11276 = DIRECTION ( 'NONE',  ( 0.000000000000000000, 0.000000000000000000, -1.000000000000000000 ) ) ;
#11277 = AXIS2_PLACEMENT_3D ( 'NONE', #14243, #11662, #17070 ) ;
#11278 = CARTESIAN_POINT ( 'NONE',  ( -38.00000000000000000, 2.000000000000000000, 0.000000000000000000 ) ) ;
#11279 = CARTESIAN_POINT ( 'NONE',  ( 20.42763382733058108, 18.00000000000000000, 24.23318166603144164 ) ) ;
#11280 = VECTOR ( 'NONE', #5696, 1000.000000000000000 ) ;
#11281 = CARTESIAN_POINT ( 'NONE',  ( -45.00000000000000711, 171.6227766016838245, 0.000000000000000000 ) ) ;
#11282 = AXIS2_PLACEMENT_3D ( 'NONE', #6865, #4119, #9678 ) ;
#11283 = ORIENTED_EDGE ( 'NONE', *, *, #4377, .F. ) ;
#11284 = DIRECTION ( 'NONE',  ( -0.000000000000000000, -0.000000000000000000, 1.000000000000000000 ) ) ;
#11285 = CARTESIAN_POINT ( 'NONE',  ( -27.98221281347037959, 19.99999999999999645, 0.000000000000000000 ) ) ;
#11286 = ORIENTED_EDGE ( 'NONE', *, *, #11900, .F. ) ;
#11287 = CARTESIAN_POINT ( 'NONE',  ( 15.00000000000000000, 154.3022685259950038, 9.999999999999900524 ) ) ;
#11288 = FACE_BOUND ( 'NONE', #11888, .T. ) ;
#11289 = EDGE_LOOP ( 'NONE', ( #2809, #3156, #16929, #17202 ) ) ;
#11290 = VERTEX_POINT ( 'NONE', #3987 ) ;
#11291 = EDGE_LOOP ( 'NONE', ( #1610, #15089, #13846, #11574 ) ) ;
#11292 = AXIS2_PLACEMENT_3D ( 'NONE', #12665, #6281, #17004 ) ;
#11293 = AXIS2_PLACEMENT_3D ( 'NONE', #7233, #12985, #3248 ) ;
#11294 = CARTESIAN_POINT ( 'NONE',  ( 9.072488053085830728, 140.2836875516620978, 12.31648485192419784 ) ) ;
#11295 = CIRCLE ( 'NONE', #11570, 2.499999999999998668 ) ;
#11296 = ORIENTED_EDGE ( 'NONE', *, *, #5854, .T. ) ;
#11297 = CIRCLE ( 'NONE', #3667, 4.000000000000002665 ) ;
#11298 = VERTEX_POINT ( 'NONE', #14774 ) ;
#11299 = CYLINDRICAL_SURFACE ( 'NONE', #10192, 5.000000000000000888 ) ;
#11300 = CARTESIAN_POINT ( 'NONE',  ( 39.99999999999998579, 0.000000000000000000, 33.00000000000000711 ) ) ;
#11301 = DIRECTION ( 'NONE',  ( 0.000000000000000000, 0.000000000000000000, -1.000000000000000000 ) ) ;
#11302 = DIRECTION ( 'NONE',  ( 0.000000000000000000, 0.000000000000000000, 1.000000000000000000 ) ) ;
#11303 = VERTEX_POINT ( 'NONE', #8033 ) ;
#11304 = CARTESIAN_POINT ( 'NONE',  ( 26.56787054652181013, 142.9736659102427723, 16.38272693053711038 ) ) ;
#11305 = AXIS2_PLACEMENT_3D ( 'NONE', #7219, #4654, #17100 ) ;
#11306 = AXIS2_PLACEMENT_3D ( 'NONE', #17156, #7762, #12918 ) ;
#11307 = CARTESIAN_POINT ( 'NONE',  ( -50.00000000000000000, 206.6227766016838245, -2.143131898507868248E-15 ) ) ;
#11308 = DIRECTION ( 'NONE',  ( -1.000000000000000000, 0.000000000000000000, 0.000000000000000000 ) ) ;
#11309 = AXIS2_PLACEMENT_3D ( 'NONE', #11226, #6894, #9544 ) ;
#11310 = CARTESIAN_POINT ( 'NONE',  ( -12.16365208422963740, 31.05675767351161909, -14.01395464075509878 ) ) ;
#11311 = SURFACE_SIDE_STYLE ('',( #6885 ) ) ;
#11312 = ADVANCED_FACE ( 'NONE', ( #13444 ), #1314, .T. ) ;
#11313 = CARTESIAN_POINT ( 'NONE',  ( -80.00000000000001421, 196.6227766016838245, 0.000000000000000000 ) ) ;
#11314 = ORIENTED_EDGE ( 'NONE', *, *, #7405, .T. ) ;
#11315 = FACE_OUTER_BOUND ( 'NONE', #7632, .T. ) ;
#11316 = AXIS2_PLACEMENT_3D ( 'NONE', #12817, #16805, #1931 ) ;
#11317 = AXIS2_PLACEMENT_3D ( 'NONE', #10697, #16112, #3986 ) ;
#11318 = ORIENTED_EDGE ( 'NONE', *, *, #12886, .T. ) ;
#11319 = SURFACE_SIDE_STYLE ('',( #15304 ) ) ;
#11320 = B_SPLINE_CURVE_WITH_KNOTS ( 'NONE', 3,
 ( #9360, #13351, #2553, #8021, #17061, #11738, #12012, #10589, #11922, #7674, #14414, #13433, #5116, #11657, #2280, #13083, #949, #10414, #3881, #7946, #15911, #3702, #14495, #17240, #2363, #7754, #13168, #9175, #1038, #6438, #11831, #14581, #7851, #13261, #11035, #6879, #1399, #12366 ),
 .UNSPECIFIED., .F., .F.,
 ( 4, 2, 2, 2, 2, 2, 2, 2, 2, 2, 2, 2, 2, 2, 2, 2, 2, 2, 4 ),
 ( 0.01870878530979003598, 0.02011211734399856454, 0.02151544937820709658, 0.02432211344662422309, 0.02572544548083275859, 0.02712877751504130103, 0.02783044353214558092, 0.02853210954924986081, 0.02923377556635414765, 0.02993544158345842754, 0.03063710760056271090, 0.03133877361766699426, 0.03204043963477128110, 0.03274210565187556099, 0.03414543768608409302, 0.03554876972029263199, 0.03695210175450117096, 0.03835543378870970299, 0.04116209785712676705 ),
 .UNSPECIFIED. ) ;
#11321 = LINE ( 'NONE', #4679, #11873 ) ;
#11322 = AXIS2_PLACEMENT_3D ( 'NONE', #4041, #16248, #6939 ) ;
#11323 = EDGE_LOOP ( 'NONE', ( #13448, #419, #11633, #16451 ) ) ;
#11324 = LINE ( 'NONE', #15569, #1662 ) ;
#11325 = CARTESIAN_POINT ( 'NONE',  ( 34.93420767853316988, 20.00000000000000000, -4.999999999999999112 ) ) ;
#11326 = CARTESIAN_POINT ( 'NONE',  ( -73.00000000000001421, 171.6227766016838245, -19.49999999999999645 ) ) ;
#11327 = VERTEX_POINT ( 'NONE', #10516 ) ;
#11328 = DIRECTION ( 'NONE',  ( 1.000000000000000000, 0.000000000000000000, 0.000000000000000000 ) ) ;
#11329 = CARTESIAN_POINT ( 'NONE',  ( -34.99999999999999289, 122.0000000000000284, 4.999999999999999112 ) ) ;
#11330 = CARTESIAN_POINT ( 'NONE',  ( -75.41000427951827589, 198.6265692133321181, 18.97388360722737843 ) ) ;
#11331 = VERTEX_POINT ( 'NONE', #5473 ) ;
#11332 = AXIS2_PLACEMENT_3D ( 'NONE', #16865, #6234, #3490 ) ;
#11333 = EDGE_CURVE ( 'NONE', #15131, #4289, #16277, .T. ) ;
#11334 = EDGE_CURVE ( 'NONE', #1967, #14287, #512, .T. ) ;
#11335 = EDGE_CURVE ( 'NONE', #5097, #9988, #15026, .T. ) ;
#11336 = ORIENTED_EDGE ( 'NONE', *, *, #15034, .T. ) ;
#11337 = CARTESIAN_POINT ( 'NONE',  ( 24.52650527911658074, 19.99999999999999645, -8.254754350130129481 ) ) ;
#11338 = CARTESIAN_POINT ( 'NONE',  ( -50.00000000000000711, -20.00000000000000000, 35.00000000000000711 ) ) ;
#11339 = EDGE_LOOP ( 'NONE', ( #7759, #13423, #9665, #1324 ) ) ;
#11340 = CARTESIAN_POINT ( 'NONE',  ( 49.99999999999998579, 159.6227766016838814, 8.071800142134975431 ) ) ;
#11341 = CARTESIAN_POINT ( 'NONE',  ( 48.00000000000000711, 175.6227766016838245, 5.571800142134975431 ) ) ;
#11342 = VERTEX_POINT ( 'NONE', #4414 ) ;
#11343 = CARTESIAN_POINT ( 'NONE',  ( 17.00000000000000000, 171.6227766016838245, 0.000000000000000000 ) ) ;
#11344 = AXIS2_PLACEMENT_3D ( 'NONE', #2534, #7926, #1379 ) ;
#11345 = CARTESIAN_POINT ( 'NONE',  ( -27.29618490519992591, 18.00000000000000000, 10.29570512375934044 ) ) ;
#11346 = DIRECTION ( 'NONE',  ( 0.000000000000000000, 0.000000000000000000, -1.000000000000000000 ) ) ;
#11347 = FACE_OUTER_BOUND ( 'NONE', #12600, .T. ) ;
#11348 = PLANE ( 'NONE',  #14463 ) ;
#11349 = DIRECTION ( 'NONE',  ( -1.000000000000000000, -0.000000000000000000, -0.000000000000000000 ) ) ;
#11350 = CARTESIAN_POINT ( 'NONE',  ( 48.00000000000000711, 167.6227766016838530, -5.571800142134975431 ) ) ;
#11351 = ORIENTED_EDGE ( 'NONE', *, *, #16954, .T. ) ;
#11352 = FACE_OUTER_BOUND ( 'NONE', #1259, .T. ) ;
#11353 = ORIENTED_EDGE ( 'NONE', *, *, #13237, .F. ) ;
#11354 = CARTESIAN_POINT ( 'NONE',  ( 39.99999999999998579, 4.000000000000007994, 33.00000000000001421 ) ) ;
#11355 = VECTOR ( 'NONE', #5511, 1000.000000000000000 ) ;
#11356 = CARTESIAN_POINT ( 'NONE',  ( 48.00000000000000711, 146.6227766016838245, -4.592425496802573578E-15 ) ) ;
#11357 = EDGE_LOOP ( 'NONE', ( #4261, #4098, #10605, #946 ) ) ;
#11358 = CARTESIAN_POINT ( 'NONE',  ( 21.38845554303141938, 19.99999999999999289, 23.94082098111162082 ) ) ;
#11359 = CARTESIAN_POINT ( 'NONE',  ( 32.29171157738787912, 19.99999999999999645, 15.02090973094133375 ) ) ;
#11360 = CARTESIAN_POINT ( 'NONE',  ( 27.42233524417435930, 136.9585154912620908, 4.953423069178740867 ) ) ;
#11361 = EDGE_LOOP ( 'NONE', ( #11562, #3027, #10640, #5799 ) ) ;
#11362 = CARTESIAN_POINT ( 'NONE',  ( 15.00000000000000000, 171.6227766016838245, 0.000000000000000000 ) ) ;
#11363 = MANIFOLD_SOLID_BREP ( 'Fillet1', #10326 ) ;
#11364 = CARTESIAN_POINT ( 'NONE',  ( -40.00000000000000000, 8.000000000000000000, -30.00000000000000711 ) ) ;
#11365 = CARTESIAN_POINT ( 'NONE',  ( -208.1430079281944074, 166.0913325906388422, 2.284806080016937635 ) ) ;
#11366 = CARTESIAN_POINT ( 'NONE',  ( 196.0000000000000000, 183.6227766016837961, -3.071800142134975431 ) ) ;
#11367 = ADVANCED_FACE ( 'NONE', ( #16543 ), #2822, .F. ) ;
#11368 = CARTESIAN_POINT ( 'NONE',  ( -31.66708739526795924, 101.0000000000000142, 5.500000000000000000 ) ) ;
#11369 = FACE_OUTER_BOUND ( 'NONE', #11361, .T. ) ;
#11370 = EDGE_CURVE ( 'NONE', #5417, #14253, #7210, .T. ) ;
#11371 = ORIENTED_EDGE ( 'NONE', *, *, #16890, .F. ) ;
#11372 = CARTESIAN_POINT ( 'NONE',  ( -32.55406425504675383, 100.5254706298719185, 5.163900856522908533 ) ) ;
#11373 = DIRECTION ( 'NONE',  ( 1.000000000000000000, -0.000000000000000000, -0.000000000000000000 ) ) ;
#11374 = EDGE_LOOP ( 'NONE', ( #4394, #7334, #7638, #16457 ) ) ;
#11375 = DIRECTION ( 'NONE',  ( 1.000000000000000000, -0.000000000000000000, -0.000000000000000000 ) ) ;
#11376 = DIRECTION ( 'NONE',  ( 0.000000000000000000, 0.000000000000000000, 1.000000000000000000 ) ) ;
#11377 = VERTEX_POINT ( 'NONE', #4324 ) ;
#11378 = ORIENTED_EDGE ( 'NONE', *, *, #2565, .F. ) ;
#11379 = ORIENTED_EDGE ( 'NONE', *, *, #15094, .T. ) ;
#11380 = ADVANCED_FACE ( 'NONE', ( #9803 ), #1493, .T. ) ;
#11381 = ORIENTED_EDGE ( 'NONE', *, *, #14888, .F. ) ;
#11382 = SURFACE_SIDE_STYLE ('',( #14138 ) ) ;
#11383 = ORIENTED_EDGE ( 'NONE', *, *, #15984, .F. ) ;
#11384 =( NAMED_UNIT ( * ) SI_UNIT ( $, .STERADIAN. ) SOLID_ANGLE_UNIT ( ) );
#11385 = CARTESIAN_POINT ( 'NONE',  ( -23.00000000000000000, 120.0000000000000284, 0.000000000000000000 ) ) ;
#11386 = CARTESIAN_POINT ( 'NONE',  ( 12.84413890157916782, 129.3215245152910313, 10.42375118840982573 ) ) ;
#11387 = CARTESIAN_POINT ( 'NONE',  ( -31.66708739526795924, 100.0000000000000142, -5.500000000000000000 ) ) ;
#11388 = CARTESIAN_POINT ( 'NONE',  ( 49.99999999999998579, 175.6227766016838530, -19.42820660268601074 ) ) ;
#11389 = ORIENTED_EDGE ( 'NONE', *, *, #7889, .T. ) ;
#11390 = CARTESIAN_POINT ( 'NONE',  ( 28.27146593557246490, 141.9273338169157341, 14.39467838667815691 ) ) ;
#11391 = DIRECTION ( 'NONE',  ( 0.000000000000000000, -0.000000000000000000, 1.000000000000000000 ) ) ;
#11392 = CYLINDRICAL_SURFACE ( 'NONE', #13877, 2.500000000000000444 ) ;
#11393 = CARTESIAN_POINT ( 'NONE',  ( -13.34744738361370509, 19.99999999999999645, -11.18154278182822026 ) ) ;
#11394 = SURFACE_STYLE_FILL_AREA ( #15470 ) ;
#11395 = ADVANCED_FACE ( 'NONE', ( #8215 ), #3560, .T. ) ;
#11396 = EDGE_CURVE ( 'NONE', #12075, #9019, #415, .T. ) ;
#11397 = CARTESIAN_POINT ( 'NONE',  ( -68.00000000000000000, 191.6227766016837961, -1.224646799147353454E-15 ) ) ;
#11398 = ORIENTED_EDGE ( 'NONE', *, *, #7429, .T. ) ;
#11399 = DIRECTION ( 'NONE',  ( -1.000000000000000000, 0.000000000000000000, 0.000000000000000000 ) ) ;
#11400 = EDGE_LOOP ( 'NONE', ( #908, #15368 ) ) ;
#11401 = LINE ( 'NONE', #14163, #14153 ) ;
#11402 = DIRECTION ( 'NONE',  ( 1.000000000000000000, 0.000000000000000000, -0.000000000000000000 ) ) ;
#11403 = EDGE_CURVE ( 'NONE', #11501, #2395, #734, .T. ) ;
#11404 = DIRECTION ( 'NONE',  ( 1.000000000000000000, 0.000000000000000000, 0.000000000000000000 ) ) ;
#11405 = VERTEX_POINT ( 'NONE', #1572 ) ;
#11406 = FACE_OUTER_BOUND ( 'NONE', #14294, .T. ) ;
#11407 = CARTESIAN_POINT ( 'NONE',  ( 27.99999999999998224, 9.999999999999998224, 0.000000000000000000 ) ) ;
#11408 = CARTESIAN_POINT ( 'NONE',  ( -76.57310389028062048, 200.2770367110204006, 16.37379161636571823 ) ) ;
#11409 = ORIENTED_EDGE ( 'NONE', *, *, #6417, .F. ) ;
#11410 = ORIENTED_EDGE ( 'NONE', *, *, #6037, .T. ) ;
#11411 = CARTESIAN_POINT ( 'NONE',  ( 21.59801423301730239, 19.99999999999999645, -12.60094170202890140 ) ) ;
#11412 = DIRECTION ( 'NONE',  ( -1.000000000000000000, 0.000000000000000000, 0.000000000000000000 ) ) ;
#11413 = ORIENTED_EDGE ( 'NONE', *, *, #16700, .F. ) ;
#11414 = LINE ( 'NONE', #6280, #3585 ) ;
#11415 = CARTESIAN_POINT ( 'NONE',  ( 7.863372401969320968, 140.4786490112420552, -12.74411896114139076 ) ) ;
#11416 = ORIENTED_EDGE ( 'NONE', *, *, #13623, .T. ) ;
#11417 = CARTESIAN_POINT ( 'NONE',  ( -103.0000000000000142, 171.6227766016838245, 0.000000000000000000 ) ) ;
#11418 = UNCERTAINTY_MEASURE_WITH_UNIT (LENGTH_MEASURE( 1.000000000000000082E-05 ), #6618, 'distance_accuracy_value', 'NONE');
#11419 = CARTESIAN_POINT ( 'NONE',  ( -13.90980987654338286, 18.00000000000000355, 23.98326992096529864 ) ) ;
#11420 = ADVANCED_FACE ( 'NONE', ( #2985 ), #8385, .F. ) ;
#11421 = EDGE_CURVE ( 'NONE', #14117, #14296, #12888, .T. ) ;
#11422 = EDGE_CURVE ( 'NONE', #5356, #3326, #16635, .T. ) ;
#11423 = CARTESIAN_POINT ( 'NONE',  ( 1.559999999999998943, -1.732050807568885631, 0.000000000000000000 ) ) ;
#11424 = CIRCLE ( 'NONE', #12842, 2.500000000000002220 ) ;
#11425 = DIRECTION ( 'NONE',  ( -0.000000000000000000, -0.000000000000000000, -1.000000000000000000 ) ) ;
#11426 = CARTESIAN_POINT ( 'NONE',  ( -11.48222079042285770, 18.00000000000000355, 9.976350980977374050 ) ) ;
#11427 = AXIS2_PLACEMENT_3D ( 'NONE', #14271, #1171, #9126 ) ;
#11428 = LINE ( 'NONE', #7103, #16254 ) ;
#11429 = CARTESIAN_POINT ( 'NONE',  ( -34.99999999999999289, 122.0000000000000284, 15.00000000000000000 ) ) ;
#11430 = VERTEX_POINT ( 'NONE', #13628 ) ;
#11431 = DIRECTION ( 'NONE',  ( 0.000000000000000000, 1.000000000000000000, 0.000000000000000000 ) ) ;
#11432 = ORIENTED_EDGE ( 'NONE', *, *, #2331, .T. ) ;
#11433 = DIRECTION ( 'NONE',  ( 0.000000000000000000, 0.000000000000000000, 1.000000000000000000 ) ) ;
#11434 = PLANE ( 'NONE',  #2998 ) ;
#11435 = VERTEX_POINT ( 'NONE', #9972 ) ;
#11436 = CARTESIAN_POINT ( 'NONE',  ( 15.00000000000000000, 171.6227766016838245, 0.000000000000000000 ) ) ;
#11437 = CIRCLE ( 'NONE', #13703, 7.500000000000000000 ) ;
#11438 = VECTOR ( 'NONE', #3293, 1000.000000000000000 ) ;
#11439 = CARTESIAN_POINT ( 'NONE',  ( 21.03709756577793399, 29.91885446100015145, 12.94894061605241831 ) ) ;
#11440 = LINE ( 'NONE', #16852, #6728 ) ;
#11441 = ORIENTED_EDGE ( 'NONE', *, *, #1487, .F. ) ;
#11442 = CONTEXT_DEPENDENT_SHAPE_REPRESENTATION ( #15117, #13511 ) ;
#11443 = EDGE_CURVE ( 'NONE', #9736, #11646, #4922, .T. ) ;
#11444 = CARTESIAN_POINT ( 'NONE',  ( -32.66708739526796279, 101.0000000000000142, 4.722170599040663497 ) ) ;
#11445 = CARTESIAN_POINT ( 'NONE',  ( 27.99999999999998224, 9.999999999999998224, -30.00000000000001066 ) ) ;
#11446 = CARTESIAN_POINT ( 'NONE',  ( -81.34794908311457107, 191.8039921295446106, 26.10980206683226967 ) ) ;
#11447 = DIRECTION ( 'NONE',  ( 0.000000000000000000, 0.000000000000000000, -1.000000000000000000 ) ) ;
#11448 = DIRECTION ( 'NONE',  ( 0.000000000000000000, 0.000000000000000000, -1.000000000000000000 ) ) ;
#11449 = CARTESIAN_POINT ( 'NONE',  ( -25.49999999999998579, 10.00000000000000000, 10.00000000000000178 ) ) ;
#11450 = CIRCLE ( 'NONE', #12869, 25.00000000000000000 ) ;
#11451 = EDGE_LOOP ( 'NONE', ( #9531, #15303 ) ) ;
#11452 = DIRECTION ( 'NONE',  ( -1.000000000000000000, -0.000000000000000000, 0.000000000000000000 ) ) ;
#11454 = CARTESIAN_POINT ( 'NONE',  ( -27.29618490519992591, 19.99999999999999645, -10.29570512375934399 ) ) ;
#11453 = STYLED_ITEM ( 'NONE', ( #14331 ), #11181 ) ;
#11455 = ORIENTED_EDGE ( 'NONE', *, *, #8737, .T. ) ;
#11456 = DIRECTION ( 'NONE',  ( 0.000000000000000000, 0.000000000000000000, -1.000000000000000000 ) ) ;
#11457 = LINE ( 'NONE', #842, #5548 ) ;
#11458 = AXIS2_PLACEMENT_3D ( 'NONE', #8132, #5743, #2994 ) ;
#11459 = EDGE_LOOP ( 'NONE', ( #4112, #10159, #12074, #870 ) ) ;
#11460 = VERTEX_POINT ( 'NONE', #10055 ) ;
#11461 = VERTEX_POINT ( 'NONE', #12815 ) ;
#11462 = EDGE_CURVE ( 'NONE', #8600, #10173, #14018, .T. ) ;
#11463 = CIRCLE ( 'NONE', #8352, 2.500000000000000444 ) ;
#11464 = VERTEX_POINT ( 'NONE', #1929 ) ;
#11465 = CYLINDRICAL_SURFACE ( 'NONE', #7369, 20.00000000000000355 ) ;
#11466 = VECTOR ( 'NONE', #3694, 1000.000000000000000 ) ;
#11467 = CARTESIAN_POINT ( 'NONE',  ( 10.69994788061133129, 131.5490474681699880, 11.88030112651796877 ) ) ;
#11468 = CIRCLE ( 'NONE', #13737, 5.000000000000000888 ) ;
#11469 = CARTESIAN_POINT ( 'NONE',  ( 4.755015822784812052, 0.000000000000000000, 0.000000000000000000 ) ) ;
#11470 = DIRECTION ( 'NONE',  ( -0.000000000000000000, -0.000000000000000000, -1.000000000000000000 ) ) ;
#11471 = ORIENTED_EDGE ( 'NONE', *, *, #15055, .F. ) ;
#11472 = CARTESIAN_POINT ( 'NONE',  ( 25.81930071191963805, 143.8651737624333578, 17.85267748742823812 ) ) ;
#11473 = LINE ( 'NONE', #17050, #273 ) ;
#11474 = FACE_OUTER_BOUND ( 'NONE', #9781, .T. ) ;
#11475 = MANIFOLD_SOLID_BREP ( 'CirPattern1[1]', #2147 ) ;
#11476 = CARTESIAN_POINT ( 'NONE',  ( -21.36854569161992856, 19.99999999999999645, -19.70709815271291632 ) ) ;
#11477 = SURFACE_SIDE_STYLE ('',( #11394 ) ) ;
#11478 = AXIS2_PLACEMENT_3D ( 'NONE', #3559, #12855, #14269 ) ;
#11479 = VECTOR ( 'NONE', #1895, 1000.000000000000000 ) ;
#11480 = CONICAL_SURFACE ( 'NONE', #6688, 2.499999999999998668, 1.029744260000002187 ) ;
#11481 = DIRECTION ( 'NONE',  ( 0.000000000000000000, 0.000000000000000000, -1.000000000000000000 ) ) ;
#11482 = VERTEX_POINT ( 'NONE', #6004 ) ;
#11483 = ADVANCED_FACE ( 'NONE', ( #14155 ), #2093, .T. ) ;
#11484 = DIRECTION ( 'NONE',  ( 0.000000000000000000, -1.000000000000000000, -1.836970198721028701E-16 ) ) ;
#11485 = ORIENTED_EDGE ( 'NONE', *, *, #6100, .F. ) ;
#11486 = PRESENTATION_STYLE_ASSIGNMENT (( #15644 ) ) ;
#11487 = CARTESIAN_POINT ( 'NONE',  ( 15.72080254704531477, 141.4281235329943343, 17.70852598599439176 ) ) ;
#11488 = CIRCLE ( 'NONE', #10644, 27.69059892324149530 ) ;
#11489 = DIRECTION ( 'NONE',  ( 0.000000000000000000, 0.000000000000000000, 1.000000000000000000 ) ) ;
#11490 = VECTOR ( 'NONE', #5317, 1000.000000000000000 ) ;
#11491 = EDGE_CURVE ( 'NONE', #10063, #1652, #4969, .T. ) ;
#11492 = CARTESIAN_POINT ( 'NONE',  ( 10.69994788061133129, 131.5490474681699880, -11.88030112651796877 ) ) ;
#11493 = EDGE_CURVE ( 'NONE', #1489, #4216, #17113, .T. ) ;
#11494 = VECTOR ( 'NONE', #2378, 1000.000000000000000 ) ;
#11495 = VERTEX_POINT ( 'NONE', #7413 ) ;
#11496 = DIRECTION ( 'NONE',  ( 1.000000000000000000, 0.000000000000000000, 0.000000000000000000 ) ) ;
#11497 = DIRECTION ( 'NONE',  ( 1.000000000000000000, 0.000000000000000000, 0.000000000000000000 ) ) ;
#11498 = CARTESIAN_POINT ( 'NONE',  ( 49.99999999999998579, 155.6227766016839098, -10.00000337241049309 ) ) ;
#11499 = CARTESIAN_POINT ( 'NONE',  ( 28.02291439894537817, 202.2921397697441819, -16.86471387523355858 ) ) ;
#11500 = ORIENTED_EDGE ( 'NONE', *, *, #12920, .T. ) ;
#11501 = VERTEX_POINT ( 'NONE', #6259 ) ;
#11502 = CARTESIAN_POINT ( 'NONE',  ( 21.98114852961611376, 19.99999999999999645, -23.72829316725777460 ) ) ;
#11503 = CARTESIAN_POINT ( 'NONE',  ( 196.0000000000000000, 179.6227766016838245, -15.00000337241049486 ) ) ;
#11504 = VECTOR ( 'NONE', #15038, 1000.000000000000000 ) ;
#11505 = EDGE_LOOP ( 'NONE', ( #536, #14135, #2082, #3471 ) ) ;
#11506 = COLOUR_RGB ( '', 0.72549020, 0.75294118, 0.79215686) ;
#11507 = CARTESIAN_POINT ( 'NONE',  ( 30.00000000000000355, 196.6227766016838245, -35.00200000000000244 ) ) ;
#11508 = AXIS2_PLACEMENT_3D ( 'NONE', #4508, #15302, #15564 ) ;
#11509 = CARTESIAN_POINT ( 'NONE',  ( -100.0000000000000000, 171.6227766016838245, -27.69059892324149175 ) ) ;
#11510 = EDGE_LOOP ( 'NONE', ( #9258, #8772, #3553 ) ) ;
#11511 = PLANE ( 'NONE',  #14700 ) ;
#11512 = CARTESIAN_POINT ( 'NONE',  ( -100.0000000000000000, 141.2912748254776147, -13.00000000000000000 ) ) ;
#11513 = CARTESIAN_POINT ( 'NONE',  ( -207.1416055535977989, 174.8004040394998526, 4.000449707837476332 ) ) ;
#11514 = CARTESIAN_POINT ( 'NONE',  ( -9.672962866393921999, 30.74839102026217574, 12.74052981562734388 ) ) ;
#11515 = CIRCLE ( 'NONE', #785, 27.69059892324149530 ) ;
#11516 = CARTESIAN_POINT ( 'NONE',  ( -125.0000000000000000, 206.6227766016838245, 0.000000000000000000 ) ) ;
#11517 =( GEOMETRIC_REPRESENTATION_CONTEXT ( 3 ) GLOBAL_UNCERTAINTY_ASSIGNED_CONTEXT ( ( #11932 ) ) GLOBAL_UNIT_ASSIGNED_CONTEXT ( ( #16549, #2910, #2742 ) ) REPRESENTATION_CONTEXT ( 'NONE', 'WORKASPACE' ) );
#11518 = CARTESIAN_POINT ( 'NONE',  ( 32.41004031834387433, 141.1235162643941408, -17.17043012754695397 ) ) ;
#11519 = ORIENTED_EDGE ( 'NONE', *, *, #11073, .F. ) ;
#11520 = CARTESIAN_POINT ( 'NONE',  ( -68.00000000000000000, 171.6227766016838245, -20.00000000000000355 ) ) ;
#11521 = VERTEX_POINT ( 'NONE', #4850 ) ;
#11522 = DIRECTION ( 'NONE',  ( -0.000000000000000000, -0.000000000000000000, -1.000000000000000000 ) ) ;
#11523 = EDGE_CURVE ( 'NONE', #12351, #11917, #16888, .T. ) ;
#11524 = DIRECTION ( 'NONE',  ( -1.156482317317868274E-16, 1.000000000000000000, 0.000000000000000000 ) ) ;
#11525 = EDGE_CURVE ( 'NONE', #8489, #6919, #8642, .T. ) ;
#11526 = ORIENTED_EDGE ( 'NONE', *, *, #17231, .T. ) ;
#11527 = CARTESIAN_POINT ( 'NONE',  ( 29.98123639043839006, 19.99999999999999645, 18.19121573219640098 ) ) ;
#11528 = CIRCLE ( 'NONE', #8705, 2.500000000000002220 ) ;
#11529 = CARTESIAN_POINT ( 'NONE',  ( 33.88365274872861477, 19.99999999999999645, 11.43011099234506212 ) ) ;
#11530 = CARTESIAN_POINT ( 'NONE',  ( 30.00000000000000355, 196.6227766016838245, 10.00000000000000178 ) ) ;
#11531 = AXIS2_PLACEMENT_3D ( 'NONE', #8224, #13636, #346 ) ;
#11532 =( GEOMETRIC_REPRESENTATION_CONTEXT ( 3 ) GLOBAL_UNCERTAINTY_ASSIGNED_CONTEXT ( ( #3463 ) ) GLOBAL_UNIT_ASSIGNED_CONTEXT ( ( #1037, #9088, #13082 ) ) REPRESENTATION_CONTEXT ( 'NONE', 'WORKASPACE' ) );
#11533 = VERTEX_POINT ( 'NONE', #2272 ) ;
#11534 = LINE ( 'NONE', #12695, #1586 ) ;
#11535 = CARTESIAN_POINT ( 'NONE',  ( 48.00000000000000000, 171.6227766016838245, 0.000000000000000000 ) ) ;
#11536 = LINE ( 'NONE', #17028, #1458 ) ;
#11537 = CARTESIAN_POINT ( 'NONE',  ( 39.99999999999998579, -20.00000000000000000, -40.00000000000001421 ) ) ;
#11538 = CARTESIAN_POINT ( 'NONE',  ( -40.00000000000000000, 0.000000000000000000, -33.00000000000000711 ) ) ;
#11539 = EDGE_LOOP ( 'NONE', ( #2695, #12365, #16595, #1003, #15993 ) ) ;
#11540 = DIRECTION ( 'NONE',  ( -1.000000000000000000, -0.000000000000000000, -0.000000000000000000 ) ) ;
#11541 = AXIS2_PLACEMENT_3D ( 'NONE', #10270, #5057, #11431 ) ;
#11542 = DIRECTION ( 'NONE',  ( 0.8571673013836870192, 1.049727191973306873E-16, -0.5150380737757234151 ) ) ;
#11543 = VERTEX_POINT ( 'NONE', #7667 ) ;
#11544 = CARTESIAN_POINT ( 'NONE',  ( -207.8765633999775275, 175.5245310743884488, -3.924903759054537478 ) ) ;
#11545 = VECTOR ( 'NONE', #15193, 1000.000000000000000 ) ;
#11546 = FACE_BOUND ( 'NONE', #2504, .T. ) ;
#11547 = EDGE_CURVE ( 'NONE', #4330, #4930, #15561, .T. ) ;
#11548 = VERTEX_POINT ( 'NONE', #11568 ) ;
#11549 = EDGE_CURVE ( 'NONE', #11634, #9311, #17053, .T. ) ;
#11550 = ORIENTED_EDGE ( 'NONE', *, *, #17518, .T. ) ;
#11551 = ADVANCED_FACE ( 'NONE', ( #944 ), #8654, .T. ) ;
#11552 = ORIENTED_EDGE ( 'NONE', *, *, #7801, .F. ) ;
#11553 = ORIENTED_EDGE ( 'NONE', *, *, #10790, .F. ) ;
#11554 = CYLINDRICAL_SURFACE ( 'NONE', #14925, 6.000000000000001776 ) ;
#11555 = VECTOR ( 'NONE', #5579, 1000.000000000000000 ) ;
#11556 = ORIENTED_EDGE ( 'NONE', *, *, #5788, .F. ) ;
#11557 = CARTESIAN_POINT ( 'NONE',  ( 24.93507336697353693, 29.86842105263157876, 0.000000000000000000 ) ) ;
#11558 = TOROIDAL_SURFACE ( 'NONE', #2515, 740.0000000000000000, 8.000000000000000000 ) ;
#11559 = CARTESIAN_POINT ( 'NONE',  ( 10.21857696054809317, 131.9747203951183110, 12.11181647197579636 ) ) ;
#11560 = DIRECTION ( 'NONE',  ( 0.000000000000000000, 0.000000000000000000, 1.000000000000000000 ) ) ;
#11561 = DIRECTION ( 'NONE',  ( 0.000000000000000000, 0.000000000000000000, 1.000000000000000000 ) ) ;
#11562 = ORIENTED_EDGE ( 'NONE', *, *, #11900, .T. ) ;
#11563 = CARTESIAN_POINT ( 'NONE',  ( 23.20616110506447072, 140.9816209840972192, 12.26578303444138207 ) ) ;
#11564 = FACE_BOUND ( 'NONE', #16064, .T. ) ;
#11565 = LINE ( 'NONE', #12813, #7930 ) ;
#11566 = ADVANCED_FACE ( 'NONE', ( #17136 ), #14067, .T. ) ;
#11567 = CARTESIAN_POINT ( 'NONE',  ( -16.77496435665412733, 32.01311153724419967, -10.06041171812362300 ) ) ;
#11568 = CARTESIAN_POINT ( 'NONE',  ( 15.56337975240373872, 125.2134999403456135, 4.999999999999997335 ) ) ;
#11569 = CIRCLE ( 'NONE', #8178, 2.500000000000000444 ) ;
#11570 = AXIS2_PLACEMENT_3D ( 'NONE', #17094, #8238, #14621 ) ;
#11571 = FACE_OUTER_BOUND ( 'NONE', #4741, .T. ) ;
#11572 = ORIENTED_EDGE ( 'NONE', *, *, #13013, .F. ) ;
#11573 = DIRECTION ( 'NONE',  ( -0.000000000000000000, -0.000000000000000000, -1.000000000000000000 ) ) ;
#11574 = ORIENTED_EDGE ( 'NONE', *, *, #6887, .T. ) ;
#11575 = FILL_AREA_STYLE ('',( #521 ) ) ;
#11576 = CARTESIAN_POINT ( 'NONE',  ( 12.22466323754103001, 142.0699085367067767, 18.75233045409083843 ) ) ;
#11577 = AXIS2_PLACEMENT_3D ( 'NONE', #14883, #12310, #16567 ) ;
#11578 = DIRECTION ( 'NONE',  ( -0.000000000000000000, -0.000000000000000000, 1.000000000000000000 ) ) ;
#11579 = CIRCLE ( 'NONE', #3967, 2.500000000000002220 ) ;
#11580 = AXIS2_PLACEMENT_3D ( 'NONE', #1151, #3803, #2382 ) ;
#11582 = DIRECTION ( 'NONE',  ( 0.000000000000000000, 0.000000000000000000, 1.000000000000000000 ) ) ;
#11581 = B_SPLINE_CURVE_WITH_KNOTS ( 'NONE', 3,
 ( #4819, #4731, #2065, #2149, #2242, #16947, #7550, #3406, #7716, #15685, #15876, #3485, #10209, #12959, #833, #6228, #3568, #2411, #9054, #10117, #13219, #11791, #17196, #11622, #16859, #8800 ),
 .UNSPECIFIED., .F., .F.,
 ( 4, 2, 2, 2, 2, 2, 2, 2, 2, 2, 2, 2, 4 ),
 ( 0.000000000000000000, 0.002066677509289960735, 0.003100016263934941754, 0.004133355018579923205, 0.006200032527869886109, 0.007233371282514866260, 0.008266710037159848146, 0.01033338754644981018, 0.01136672630109478513, 0.01240006505573976354, 0.01446674256502970997, 0.01550008131967467971, 0.01653342007431965119 ),
 .UNSPECIFIED. ) ;
#11583 = EDGE_LOOP ( 'NONE', ( #15942, #2612, #16217, #16107 ) ) ;
#11584 = CARTESIAN_POINT ( 'NONE',  ( -25.00000000000002132, 130.0000000000000000, -15.00000000000000000 ) ) ;
#11585 = DIRECTION ( 'NONE',  ( 0.000000000000000000, 1.387778780781445676E-14, -1.000000000000000000 ) ) ;
#11586 = ADVANCED_FACE ( 'NONE', ( #1390 ), #2543, .F. ) ;
#11587 = CARTESIAN_POINT ( 'NONE',  ( -34.99999999999999289, 130.0000000000000000, 0.000000000000000000 ) ) ;
#11588 = EDGE_CURVE ( 'NONE', #13136, #12617, #3773, .T. ) ;
#11589 = CARTESIAN_POINT ( 'NONE',  ( 32.97919343609721921, 201.8349995435116568, -17.67084604013262705 ) ) ;
#11590 = ORIENTED_EDGE ( 'NONE', *, *, #5921, .T. ) ;
#11591 = VERTEX_POINT ( 'NONE', #17227 ) ;
#11592 = CARTESIAN_POINT ( 'NONE',  ( 17.52239125723112778, 29.96525225773407186, -14.66037399604394942 ) ) ;
#11593 = CIRCLE ( 'NONE', #17254, 250.0000000000000000 ) ;
#11594 = DIRECTION ( 'NONE',  ( -1.000000000000000000, -0.000000000000000000, -0.000000000000000000 ) ) ;
#11595 = ORIENTED_EDGE ( 'NONE', *, *, #8453, .T. ) ;
#11596 = CARTESIAN_POINT ( 'NONE',  ( -100.0000000000000000, 171.6227766016838245, 0.000000000000000000 ) ) ;
#11597 = CIRCLE ( 'NONE', #12175, 8.000000000000000000 ) ;
#11598 = EDGE_CURVE ( 'NONE', #15841, #14845, #7841, .T. ) ;
#11599 = LINE ( 'NONE', #8929, #12892 ) ;
#11600 = ORIENTED_EDGE ( 'NONE', *, *, #6080, .F. ) ;
#11601 = DIRECTION ( 'NONE',  ( 1.000000000000000000, 0.000000000000000000, 0.000000000000000000 ) ) ;
#11602 = CYLINDRICAL_SURFACE ( 'NONE', #6393, 2.500000000000000444 ) ;
#11603 = CYLINDRICAL_SURFACE ( 'NONE', #8050, 6.000000000000005329 ) ;
#11604 = VECTOR ( 'NONE', #11018, 1000.000000000000000 ) ;
#11605 = CARTESIAN_POINT ( 'NONE',  ( -11.99122994684827503, 18.00000000000000000, 24.50500383881282573 ) ) ;
#11606 = DIRECTION ( 'NONE',  ( 0.000000000000000000, 0.000000000000000000, -1.000000000000000000 ) ) ;
#11607 = CIRCLE ( 'NONE', #6242, 2.500000000000002220 ) ;
#11608 = LINE ( 'NONE', #7702, #6649 ) ;
#11609 = ORIENTED_EDGE ( 'NONE', *, *, #8585, .F. ) ;
#11610 = CARTESIAN_POINT ( 'NONE',  ( 49.99999999999998579, 167.6227766016838814, -21.92820660268601074 ) ) ;
#11611 = ORIENTED_EDGE ( 'NONE', *, *, #1642, .T. ) ;
#11612 = PLANE ( 'NONE',  #9305 ) ;
#11613 = PRODUCT_RELATED_PRODUCT_CATEGORY ( 'part', '', ( #1494 ) ) ;
#11614 = CARTESIAN_POINT ( 'NONE',  ( -153.0000000000000284, 196.6227766016838245, 0.000000000000000000 ) ) ;
#11615 = ORIENTED_EDGE ( 'NONE', *, *, #12350, .T. ) ;
#11616 = DIRECTION ( 'NONE',  ( 0.000000000000000000, 0.000000000000000000, 1.000000000000000000 ) ) ;
#11617 = EDGE_CURVE ( 'NONE', #6590, #7472, #16089, .T. ) ;
#11618 = CIRCLE ( 'NONE', #6544, 10.00000000000000178 ) ;
#11619 = CARTESIAN_POINT ( 'NONE',  ( 29.97257796258477569, 19.99999999999999645, 18.20111186907413270 ) ) ;
#11620 = EDGE_LOOP ( 'NONE', ( #3739, #15950, #2803, #10479 ) ) ;
#11621 = LINE ( 'NONE', #11693, #5260 ) ;
#11622 = CARTESIAN_POINT ( 'NONE',  ( -18.23240235453911140, 32.30379688028049401, -5.697301546657946858 ) ) ;
#11623 = ADVANCED_FACE ( 'NONE', ( #15990, #7937 ), #59, .T. ) ;
#11624 = DIRECTION ( 'NONE',  ( 0.000000000000000000, 0.000000000000000000, 1.000000000000000000 ) ) ;
#11625 = ORIENTED_EDGE ( 'NONE', *, *, #8652, .F. ) ;
#11626 = DIRECTION ( 'NONE',  ( 0.000000000000000000, 0.000000000000000000, 1.000000000000000000 ) ) ;
#11627 = VECTOR ( 'NONE', #13600, 1000.000000000000000 ) ;
#11628 = CARTESIAN_POINT ( 'NONE',  ( -86.00000000000001421, 196.6227766016838245, -24.49489742783178770 ) ) ;
#11629 = ORIENTED_EDGE ( 'NONE', *, *, #10648, .T. ) ;
#11630 = CARTESIAN_POINT ( 'NONE',  ( 28.21992570506699494, 190.8885537947572573, -29.22050223063088481 ) ) ;
#11631 = CARTESIAN_POINT ( 'NONE',  ( -23.00000000000001421, 122.0000000000000284, -4.999999999999999112 ) ) ;
#11632 = ORIENTED_EDGE ( 'NONE', *, *, #11923, .T. ) ;
#11633 = ORIENTED_EDGE ( 'NONE', *, *, #2304, .F. ) ;
#11634 = VERTEX_POINT ( 'NONE', #2442 ) ;
#11635 = CARTESIAN_POINT ( 'NONE',  ( 196.0000000000000000, 151.6227766016839098, 3.071800142134974099 ) ) ;
#11636 = ORIENTED_EDGE ( 'NONE', *, *, #16170, .F. ) ;
#11637 = DIRECTION ( 'NONE',  ( 0.000000000000000000, 0.000000000000000000, 1.000000000000000000 ) ) ;
#11638 = CARTESIAN_POINT ( 'NONE',  ( 196.0000000000000000, 155.6227766016839098, -12.50000337241049309 ) ) ;
#11639 =( BOUNDED_CURVE ( )  B_SPLINE_CURVE ( 3, ( #16966, #8636, #15189, #7138 ),
 .UNSPECIFIED., .F., .F. ) 
 B_SPLINE_CURVE_WITH_KNOTS ( ( 4, 4 ),
 ( 2.005774019098183203E-15, 1.490556265852237994 ),
 .UNSPECIFIED. ) 
 CURVE ( )  GEOMETRIC_REPRESENTATION_ITEM ( )  RATIONAL_B_SPLINE_CURVE ( ( 1.000000000000000000, 0.8232662051119118418, 0.8232662051119118418, 1.000000000000000000 ) ) 
 REPRESENTATION_ITEM ( '' )  );
#11640 = CYLINDRICAL_SURFACE ( 'NONE', #264, 5.000000000000004441 ) ;
#11641 = EDGE_CURVE ( 'NONE', #9733, #4462, #11914, .T. ) ;
#11642 = DIRECTION ( 'NONE',  ( -1.000000000000000000, 0.000000000000000000, 0.000000000000000000 ) ) ;
#11643 = EDGE_CURVE ( 'NONE', #16355, #1583, #17319, .T. ) ;
#11644 = DIRECTION ( 'NONE',  ( 0.9961946980917465444, 0.08715574274764831264, 0.000000000000000000 ) ) ;
#11645 = EDGE_CURVE ( 'NONE', #12308, #12465, #5107, .T. ) ;
#11646 = VERTEX_POINT ( 'NONE', #3872 ) ;
#11647 = CARTESIAN_POINT ( 'NONE',  ( -80.00000000000002842, 146.6227766016838245, 0.000000000000000000 ) ) ;
#11648 = DIRECTION ( 'NONE',  ( 1.000000000000000000, -0.000000000000000000, -0.000000000000000000 ) ) ;
#11649 = CARTESIAN_POINT ( 'NONE',  ( -44.99999999999997868, -20.00000000000000000, -40.00000000000000000 ) ) ;
#11650 = CARTESIAN_POINT ( 'NONE',  ( 39.99999999999998579, 8.000000000000007105, 30.00000000000001066 ) ) ;
#11651 = CARTESIAN_POINT ( 'NONE',  ( -85.00000000000002842, 196.6227766016838245, -35.00200000000000244 ) ) ;
#11652 = CARTESIAN_POINT ( 'NONE',  ( -40.00000000000000000, 4.000000000000007994, 33.00000000000001421 ) ) ;
#11653 = ORIENTED_EDGE ( 'NONE', *, *, #13790, .T. ) ;
#11654 = SURFACE_STYLE_USAGE ( .BOTH. , #9171 ) ;
#11655 = CARTESIAN_POINT ( 'NONE',  ( -138.7106781186547266, 171.6227766016838245, -2.296212748401287183E-15 ) ) ;
#11656 = EDGE_LOOP ( 'NONE', ( #12184, #4279, #298, #13673, #11088 ) ) ;
#11657 = CARTESIAN_POINT ( 'NONE',  ( -78.28305234797585399, 141.9230918234059686, 14.38591257614910468 ) ) ;
#11658 = LINE ( 'NONE', #4857, #2215 ) ;
#11659 = DIRECTION ( 'NONE',  ( -0.000000000000000000, -0.000000000000000000, 1.000000000000000000 ) ) ;
#11660 = VERTEX_POINT ( 'NONE', #9352 ) ;
#11661 = DIRECTION ( 'NONE',  ( -1.000000000000000000, 0.000000000000000000, 0.000000000000000000 ) ) ;
#11662 = DIRECTION ( 'NONE',  ( -0.000000000000000000, -0.000000000000000000, 1.000000000000000000 ) ) ;
#11663 = DIRECTION ( 'NONE',  ( -1.000000000000000000, -0.000000000000000000, -0.000000000000000000 ) ) ;
#11664 = CARTESIAN_POINT ( 'NONE',  ( 34.99288146128931487, 199.9683764595548610, -20.53727899274374380 ) ) ;
#11665 = ORIENTED_EDGE ( 'NONE', *, *, #4504, .T. ) ;
#11666 = ORIENTED_EDGE ( 'NONE', *, *, #12889, .F. ) ;
#11667 = CARTESIAN_POINT ( 'NONE',  ( 17.20299680575017831, 29.96951112202298262, -14.74034971990100296 ) ) ;
#11668 = CARTESIAN_POINT ( 'NONE',  ( 9.986687348566183786, 132.8041431104223307, -14.33374896416919064 ) ) ;
#11669 = EDGE_LOOP ( 'NONE', ( #4638, #3965, #12654, #2041 ) ) ;
#11670 = FACE_OUTER_BOUND ( 'NONE', #15254, .T. ) ;
#11671 = DIRECTION ( 'NONE',  ( 0.000000000000000000, 0.000000000000000000, 1.000000000000000000 ) ) ;
#11672 = EDGE_LOOP ( 'NONE', ( #10989, #519 ) ) ;
#11673 = CARTESIAN_POINT ( 'NONE',  ( 48.00000000000000711, 155.6227766016839098, -12.50000337241049309 ) ) ;
#11674 = EDGE_CURVE ( 'NONE', #2616, #12728, #10680, .T. ) ;
#11675 = CIRCLE ( 'NONE', #1215, 5.000000000000000888 ) ;
#11676 = DIRECTION ( 'NONE',  ( -1.000000000000000000, -0.000000000000000000, -0.000000000000000000 ) ) ;
#11677 = DIRECTION ( 'NONE',  ( -0.000000000000000000, -0.000000000000000000, 1.000000000000000000 ) ) ;
#11678 = CARTESIAN_POINT ( 'NONE',  ( -13.91527097789399292, 18.00000000000000000, 23.98152295253420618 ) ) ;
#11679 = DIRECTION ( 'NONE',  ( 1.000000000000000000, -0.000000000000000000, -0.000000000000000000 ) ) ;
#11680 = DIRECTION ( 'NONE',  ( 0.000000000000000000, 0.000000000000000000, 1.000000000000000000 ) ) ;
#11681 = VERTEX_POINT ( 'NONE', #17505 ) ;
#11682 = LINE ( 'NONE', #16930, #9567 ) ;
#11683 = ORIENTED_EDGE ( 'NONE', *, *, #10374, .F. ) ;
#11684 = DIRECTION ( 'NONE',  ( 0.000000000000000000, 0.000000000000000000, -1.000000000000000000 ) ) ;
#11685 = DIRECTION ( 'NONE',  ( -1.000000000000000000, -6.938893903907228378E-16, 0.000000000000000000 ) ) ;
#11686 = ORIENTED_EDGE ( 'NONE', *, *, #16708, .F. ) ;
#11687 = CARTESIAN_POINT ( 'NONE',  ( 32.91012024024373517, 19.99999999999999289, 13.86436652238006673 ) ) ;
#11688 = CARTESIAN_POINT ( 'NONE',  ( 24.72170379509201865, 19.99999999999999289, 7.619165077983454104 ) ) ;
#11689 = EDGE_CURVE ( 'NONE', #1773, #16806, #6317, .T. ) ;
#11690 = AXIS2_PLACEMENT_3D ( 'NONE', #17067, #3706, #9092 ) ;
#11691 = ORIENTED_EDGE ( 'NONE', *, *, #3514, .T. ) ;
#11692 = AXIS2_PLACEMENT_3D ( 'NONE', #13758, #11090, #3211 ) ;
#11693 = CARTESIAN_POINT ( 'NONE',  ( 25.00000000000000711, 146.6227766016838245, -35.00200000000000244 ) ) ;
#11694 = CARTESIAN_POINT ( 'NONE',  ( 24.37944869002583914, 191.6508168144186186, -26.22852547856965444 ) ) ;
#11695 = EDGE_CURVE ( 'NONE', #1696, #1803, #7747, .T. ) ;
#11696 = CARTESIAN_POINT ( 'NONE',  ( 17.00000000000000000, 171.6227766016838245, -20.00000000000000355 ) ) ;
#11697 = CARTESIAN_POINT ( 'NONE',  ( -11.48222079042285770, 17.99999999999884182, -9.976350980977374050 ) ) ;
#11698 = EDGE_CURVE ( 'NONE', #13265, #12106, #16571, .T. ) ;
#11699 = ADVANCED_FACE ( 'NONE', ( #11822 ), #14833, .T. ) ;
#11700 = ORIENTED_EDGE ( 'NONE', *, *, #10313, .F. ) ;
#11701 = CARTESIAN_POINT ( 'NONE',  ( -23.00000000000000000, 120.0000000000000284, 0.000000000000000000 ) ) ;
#11702 = ORIENTED_EDGE ( 'NONE', *, *, #13896, .F. ) ;
#11703 = CARTESIAN_POINT ( 'NONE',  ( 24.13852584367151266, 195.3295718346067531, -25.74952675241122080 ) ) ;
#11704 = CARTESIAN_POINT ( 'NONE',  ( 30.00000000000001066, 146.6227766016838245, 0.000000000000000000 ) ) ;
#11705 = AXIS2_PLACEMENT_3D ( 'NONE', #4280, #9661, #4358 ) ;
#11706 = B_SPLINE_CURVE_WITH_KNOTS ( 'NONE', 3,
 ( #14868, #6735, #14784, #1334, #16128, #2658, #12136, #8049, #88, #1425, #6, #4077, #17445, #9457, #5577, #2748, #6825, #12217, #5487, #14703, #15037, #10873, #10968, #16293, #9548 ),
 .UNSPECIFIED., .F., .F.,
 ( 4, 2, 2, 1, 2, 2, 2, 2, 2, 2, 2, 2, 4 ),
 ( 0.000000000000000000, 0.003937549356687076833, 0.005906324035030613949, 0.007875098713374151932, 0.009843873391717689048, 0.01181264807006122616, 0.01575019742674830733, 0.01771897210509184445, 0.01968774678343538503, 0.02362529614012245927, 0.02559407081846599985, 0.02756284549680953697, 0.03150039485349661467 ),
 .UNSPECIFIED. ) ;
#11707 = ORIENTED_EDGE ( 'NONE', *, *, #13053, .T. ) ;
#11708 = EDGE_CURVE ( 'NONE', #6176, #11377, #2140, .T. ) ;
#11709 = AXIS2_PLACEMENT_3D ( 'NONE', #6744, #16032, #5492 ) ;
#11710 = EDGE_LOOP ( 'NONE', ( #9953, #10852 ) ) ;
#11711 = ORIENTED_EDGE ( 'NONE', *, *, #13570, .F. ) ;
#11712 = EDGE_CURVE ( 'NONE', #15641, #1170, #12615, .T. ) ;
#11713 = CARTESIAN_POINT ( 'NONE',  ( -73.52759457847471936, 150.4190785964221106, -25.28784208911848452 ) ) ;
#11714 = ORIENTED_EDGE ( 'NONE', *, *, #6382, .T. ) ;
#11715 = CARTESIAN_POINT ( 'NONE',  ( 32.50000000000000711, 146.6227766016838245, 10.00000000000000178 ) ) ;
#11716 = CIRCLE ( 'NONE', #4109, 8.000000000000000000 ) ;
#11717 = CARTESIAN_POINT ( 'NONE',  ( 28.41545104427121515, 152.4141840272156401, -29.25805444611330230 ) ) ;
#11718 = CARTESIAN_POINT ( 'NONE',  ( 23.03715179780268585, 17.99999999999999645, 6.069068567132035241 ) ) ;
#11719 = DIRECTION ( 'NONE',  ( 0.9961946980917463224, -0.04357787137382344855, -0.07547908730516518505 ) ) ;
#11720 = EDGE_LOOP ( 'NONE', ( #12429, #13928, #6167, #3439 ) ) ;
#11721 = CARTESIAN_POINT ( 'NONE',  ( -80.00000000000002842, 146.6227766016838245, 10.00000000000000178 ) ) ;
#11722 = CARTESIAN_POINT ( 'NONE',  ( 23.07174175064647059, 29.89240369784053897, -10.82181213433699618 ) ) ;
#11723 = PLANE ( 'NONE',  #8488 ) ;
#11724 = CARTESIAN_POINT ( 'NONE',  ( 15.59275333247216366, 29.99107914678833353, 15.00000000000000000 ) ) ;
#11725 = ORIENTED_EDGE ( 'NONE', *, *, #3171, .F. ) ;
#11726 = DIRECTION ( 'NONE',  ( -0.08715574274765379437, 0.9961946980917459893, 0.000000000000000000 ) ) ;
#11727 = CARTESIAN_POINT ( 'NONE',  ( 33.63737915383075716, 200.0658281092903223, 16.73852573662798804 ) ) ;
#11728 = EDGE_CURVE ( 'NONE', #9320, #14218, #14298, .T. ) ;
#11729 = EDGE_CURVE ( 'NONE', #2572, #6776, #1555, .T. ) ;
#11730 = VECTOR ( 'NONE', #3601, 1000.000000000000000 ) ;
#11731 = EDGE_CURVE ( 'NONE', #5020, #5464, #8918, .T. ) ;
#11732 = ORIENTED_EDGE ( 'NONE', *, *, #3616, .F. ) ;
#11733 = CARTESIAN_POINT ( 'NONE',  ( -32.66708739526796990, 100.9060348297503964, -4.814896201975306766 ) ) ;
#11734 = AXIS2_PLACEMENT_3D ( 'NONE', #11388, #14146, #6075 ) ;
#11735 = DIRECTION ( 'NONE',  ( -1.000000000000000000, -0.000000000000000000, -0.000000000000000000 ) ) ;
#11736 =( BOUNDED_SURFACE ( )  B_SPLINE_SURFACE ( 3, 2, ( 
 ( #3349, #7412, #7326 ),
 ( #12302, #1928, #5914 ),
 ( #606, #511, #6903 ),
 ( #2921, #8824, #8310 ),
 ( #12735, #13726, #15373 ),
 ( #16981, #10236, #6081 ),
 ( #9644, #14230, #10054 ),
 ( #11310, #3250, #16724 ),
 ( #8653, #9971, #2018 ),
 ( #6003, #4590, #1596 ),
 ( #8744, #14154, #10976 ),
 ( #3433, #11393, #4668 ),
 ( #15469, #685, #11476 ),
 ( #6999, #4763, #10150 ),
 ( #15560, #2092, #7488 ),
 ( #12900, #776, #6171 ),
 ( #11567, #4849, #15043 ),
 ( #15634, #8236, #13643 ),
 ( #1509, #4262, #5186 ),
 ( #3692, #12987, #6331 ),
 ( #1119, #17317, #3599 ),
 ( #6522, #867, #9165 ),
 ( #13075, #14571, #13250 ),
 ( #5105, #7579, #10401 ) ),
 .UNSPECIFIED., .F., .F., .F. ) 
 B_SPLINE_SURFACE_WITH_KNOTS ( ( 4, 2, 2, 2, 2, 2, 2, 2, 2, 2, 2, 4 ),
 ( 3, 3 ),
 ( 0.01427588378380419132, 0.01824401167166925936, 0.02022807561560179684, 0.02221213955953433086, 0.02618026744739940237, 0.02816433139133193639, 0.03014839533526447041, 0.03411652322312953844, 0.03610058716706207593, 0.03808465111099461342, 0.04205277899885968146, 0.04602090688672474950 ),
 ( 0.000000000000000000, 1.000000000000000000 ),
 .UNSPECIFIED. ) 
 GEOMETRIC_REPRESENTATION_ITEM ( )  RATIONAL_B_SPLINE_SURFACE ( (
 ( 1.000000000000000000, 0.7071067811865476838, 1.000000000000000000),
 ( 1.000000000000000000, 0.7013659285814082267, 1.000000000000000000),
 ( 1.000000000000000000, 0.6957352470443716186, 1.000000000000000000),
 ( 1.000000000000000000, 0.6874449304735253952, 1.000000000000000000),
 ( 1.000000000000000000, 0.6847075230359779274, 1.000000000000000000),
 ( 1.000000000000000000, 0.6792848743381553200, 1.000000000000000000),
 ( 1.000000000000000000, 0.6765866164121365767, 1.000000000000000000),
 ( 1.000000000000000000, 0.6687223666254397125, 1.000000000000000000),
 ( 1.000000000000000000, 0.6637534122518267132, 1.000000000000000000),
 ( 1.000000000000000000, 0.6567012635110727192, 1.000000000000000000),
 ( 1.000000000000000000, 0.6544178910915308123, 1.000000000000000000),
 ( 1.000000000000000000, 0.6499901663949341213, 1.000000000000000000),
 ( 1.000000000000000000, 0.6478648508491323676, 1.000000000000000000),
 ( 1.000000000000000000, 0.6418284244073564349, 1.000000000000000000),
 ( 1.000000000000000000, 0.6382188548936990058, 1.000000000000000000),
 ( 1.000000000000000000, 0.6334349500989927551, 1.000000000000000000),
 ( 1.000000000000000000, 0.6319385063094495880, 1.000000000000000000),
 ( 1.000000000000000000, 0.6292162870119188955, 1.000000000000000000),
 ( 1.000000000000000000, 0.6279881568154176419, 1.000000000000000000),
 ( 1.000000000000000000, 0.6246939197237179053, 1.000000000000000000),
 ( 1.000000000000000000, 0.6230139244305938906, 1.000000000000000000),
 ( 1.000000000000000000, 0.6207349535630983794, 1.000000000000000000),
 ( 1.000000000000000000, 0.6201739322037901347, 1.000000000000000000),
 ( 1.000000000000000000, 0.6201736729460421982, 1.000000000000000000) ) ) 
 REPRESENTATION_ITEM ( '' )  SURFACE ( )  );
#11737 = VERTEX_POINT ( 'NONE', #16353 ) ;
#11738 = CARTESIAN_POINT ( 'NONE',  ( -75.51110111240549827, 144.3473407286824681, 18.59810793231919845 ) ) ;
#11739 = CARTESIAN_POINT ( 'NONE',  ( -19.68629150101526903, 125.3137084989847807, -12.99999999999998401 ) ) ;
#11740 = DIRECTION ( 'NONE',  ( 0.000000000000000000, 0.000000000000000000, -1.000000000000000000 ) ) ;
#11741 = CARTESIAN_POINT ( 'NONE',  ( -38.00000000000000000, 2.000000000000000000, 0.000000000000000000 ) ) ;
#11742 = TOROIDAL_SURFACE ( 'NONE', #6110, 25.00000000000000000, 8.000000000000000000 ) ;
#11743 = ORIENTED_EDGE ( 'NONE', *, *, #6037, .F. ) ;
#11744 = CYLINDRICAL_SURFACE ( 'NONE', #3895, 25.69059892324149175 ) ;
#11745 = DIRECTION ( 'NONE',  ( 0.000000000000000000, 0.000000000000000000, 1.000000000000000000 ) ) ;
#11746 = CIRCLE ( 'NONE', #6383, 30.00000000000000000 ) ;
#11747 = CARTESIAN_POINT ( 'NONE',  ( -103.0000000000000142, 171.6227766016838245, -6.000000000000005329 ) ) ;
#11748 = CARTESIAN_POINT ( 'NONE',  ( 24.00000000000000355, 196.8086972563010022, -24.30514295430832306 ) ) ;
#11749 = EDGE_LOOP ( 'NONE', ( #4486, #3257, #13747, #12965, #16751 ) ) ;
#11750 = CIRCLE ( 'NONE', #11458, 3.999999999999985789 ) ;
#11751 = VERTEX_POINT ( 'NONE', #13779 ) ;
#11752 = CYLINDRICAL_SURFACE ( 'NONE', #5240, 5.000000000000004441 ) ;
#11753 = EDGE_LOOP ( 'NONE', ( #5088, #3497 ) ) ;
#11754 = CARTESIAN_POINT ( 'NONE',  ( 15.42236477930650906, 141.4984257577436892, -17.82510376534603580 ) ) ;
#11755 = EDGE_CURVE ( 'NONE', #5268, #5381, #9475, .T. ) ;
#11756 = ADVANCED_FACE ( 'NONE', ( #140 ), #4221, .T. ) ;
#11757 = EDGE_LOOP ( 'NONE', ( #16809, #9087, #1397, #12053 ) ) ;
#11758 = CARTESIAN_POINT ( 'NONE',  ( 196.0000000000000000, 171.6227766016838245, -10.00000337241048953 ) ) ;
#11759 = CARTESIAN_POINT ( 'NONE',  ( 14.63750484765316706, 138.5418767416829837, -5.508738673615532377 ) ) ;
#11760 = AXIS2_PLACEMENT_3D ( 'NONE', #5953, #16833, #11346 ) ;
#11761 = EDGE_LOOP ( 'NONE', ( #13734, #12081, #4207, #15357 ) ) ;
#11762 = VECTOR ( 'NONE', #10210, 1000.000000000000000 ) ;
#11763 = CARTESIAN_POINT ( 'NONE',  ( 225.0000000000000000, 89.99999999999997158, 4.999999999999999112 ) ) ;
#11764 = FACE_BOUND ( 'NONE', #14054, .T. ) ;
#11765 = CARTESIAN_POINT ( 'NONE',  ( 33.76178337805616536, 193.3250171236886388, 24.86042266551077518 ) ) ;
#11766 = CARTESIAN_POINT ( 'NONE',  ( -45.00000000000001421, 8.000000000000000000, 35.00000000000000711 ) ) ;
#11767 = DIRECTION ( 'NONE',  ( 0.000000000000000000, -1.000000000000000000, 0.000000000000000000 ) ) ;
#11768 = CARTESIAN_POINT ( 'NONE',  ( -11.61061639343520824, 17.99999999999999645, 9.781492982398956926 ) ) ;
#11769 = FACE_OUTER_BOUND ( 'NONE', #2763, .T. ) ;
#11770 = CARTESIAN_POINT ( 'NONE',  ( -23.00000000000000000, 120.0000000000000284, -4.999999999999999112 ) ) ;
#11771 = CIRCLE ( 'NONE', #6408, 2.500000000000000444 ) ;
#11772 = EDGE_LOOP ( 'NONE', ( #11519, #14241, #13468, #12419 ) ) ;
#11773 = CARTESIAN_POINT ( 'NONE',  ( 196.0000000000000000, 167.6227766016838530, -5.571800142134975431 ) ) ;
#11774 = VECTOR ( 'NONE', #11642, 1000.000000000000000 ) ;
#11775 = ORIENTED_EDGE ( 'NONE', *, *, #14312, .F. ) ;
#11776 = EDGE_CURVE ( 'NONE', #6665, #16876, #12531, .T. ) ;
#11777 = AXIS2_PLACEMENT_3D ( 'NONE', #6596, #13140, #7653 ) ;
#11778 = DIRECTION ( 'NONE',  ( -1.000000000000000000, 0.000000000000000000, 0.000000000000000000 ) ) ;
#11779 = AXIS2_PLACEMENT_3D ( 'NONE', #14339, #2209, #3995 ) ;
#11780 = CARTESIAN_POINT ( 'NONE',  ( -23.65835920965563233, 18.00000000000000000, -17.33937328557891533 ) ) ;
#11781 = ORIENTED_EDGE ( 'NONE', *, *, #15931, .T. ) ;
#11782 = CARTESIAN_POINT ( 'NONE',  ( 48.00000000000000711, 163.6227766016838530, -12.50000337241049309 ) ) ;
#11783 = CARTESIAN_POINT ( 'NONE',  ( 14.28882419134376747, 138.6263508161794675, 3.987386623658552232 ) ) ;
#11784 = DIRECTION ( 'NONE',  ( 1.000000000000000000, 0.000000000000000000, 0.000000000000000000 ) ) ;
#11785 = ORIENTED_EDGE ( 'NONE', *, *, #15870, .F. ) ;
#11786 = AXIS2_PLACEMENT_3D ( 'NONE', #428, #7679, #14589 ) ;
#11787 = PRODUCT_DEFINITION_FORMATION_WITH_SPECIFIED_SOURCE ( 'ANY', '', #15205, .NOT_KNOWN. ) ;
#11788 = DIRECTION ( 'NONE',  ( -0.000000000000000000, -0.000000000000000000, 1.000000000000000000 ) ) ;
#11789 = CIRCLE ( 'NONE', #1070, 2.499999999999998668 ) ;
#11790 = CARTESIAN_POINT ( 'NONE',  ( 22.52785494716452419, 195.8611292878214272, -22.40167687543583952 ) ) ;
#11791 = CARTESIAN_POINT ( 'NONE',  ( -18.09555036921010540, 32.27673591576833445, -6.733025906873759681 ) ) ;
#11792 = CARTESIAN_POINT ( 'NONE',  ( -13.23954943057894873, 31.86042443463173157, -11.05847410484002680 ) ) ;
#11793 = EDGE_LOOP ( 'NONE', ( #6160, #4750, #2104, #4154 ) ) ;
#11794 = DIRECTION ( 'NONE',  ( 0.000000000000000000, 1.000000000000000000, 0.000000000000000000 ) ) ;
#11795 = ORIENTED_EDGE ( 'NONE', *, *, #3884, .F. ) ;
#11796 = ADVANCED_FACE ( 'NONE', ( #16446 ), #15276, .F. ) ;
#11797 = CARTESIAN_POINT ( 'NONE',  ( 31.13603083703002383, 190.7269353522202664, -29.32635129980145194 ) ) ;
#11798 = DIRECTION ( 'NONE',  ( 1.000000000000000000, 0.000000000000000000, 0.000000000000000000 ) ) ;
#11799 = VERTEX_POINT ( 'NONE', #1478 ) ;
#11800 = VECTOR ( 'NONE', #5818, 1000.000000000000000 ) ;
#11801 = VERTEX_POINT ( 'NONE', #9606 ) ;
#11802 = VERTEX_POINT ( 'NONE', #4309 ) ;
#11803 = ADVANCED_FACE ( 'NONE', ( #12266 ), #9689, .T. ) ;
#11804 = CARTESIAN_POINT ( 'NONE',  ( -87.50000000000004263, 146.6227766016838245, -21.54065922853802562 ) ) ;
#11805 = UNCERTAINTY_MEASURE_WITH_UNIT (LENGTH_MEASURE( 1.000000000000000082E-05 ), #777, 'distance_accuracy_value', 'NONE');
#11806 = EDGE_CURVE ( 'NONE', #8380, #6279, #15087, .T. ) ;
#11807 = ORIENTED_EDGE ( 'NONE', *, *, #2565, .T. ) ;
#11808 = DIRECTION ( 'NONE',  ( 0.000000000000000000, 0.000000000000000000, 1.000000000000000000 ) ) ;
#11809 = CYLINDRICAL_SURFACE ( 'NONE', #6521, 2.500000000000000444 ) ;
#11810 = DIRECTION ( 'NONE',  ( -0.000000000000000000, -0.000000000000000000, -1.000000000000000000 ) ) ;
#11811 = CARTESIAN_POINT ( 'NONE',  ( 32.29171157743327569, 18.00000000000000000, 15.02090973096405158 ) ) ;
#11812 = CARTESIAN_POINT ( 'NONE',  ( -85.00000000000002842, 146.6227766016838245, 21.54065922853802562 ) ) ;
#11813 = CIRCLE ( 'NONE', #5888, 2.500000000000002220 ) ;
#11814 = CIRCLE ( 'NONE', #9269, 27.69059892324149175 ) ;
#11815 = ORIENTED_EDGE ( 'NONE', *, *, #10670, .F. ) ;
#11816 = CARTESIAN_POINT ( 'NONE',  ( 30.00000000000001066, 146.6227766016838245, -35.00200000000000244 ) ) ;
#11817 = CARTESIAN_POINT ( 'NONE',  ( 14.93242934743711992, 30.00000000000000000, -15.00000000000000000 ) ) ;
#11818 = DIRECTION ( 'NONE',  ( -1.000000000000000000, 0.000000000000000000, 0.000000000000000000 ) ) ;
#11819 = CARTESIAN_POINT ( 'NONE',  ( 34.42405209918207731, 18.00000000000000000, 9.535225002503356251 ) ) ;
#11820 = FACE_BOUND ( 'NONE', #853, .T. ) ;
#11821 = EDGE_LOOP ( 'NONE', ( #3766, #10756 ) ) ;
#11822 = FACE_OUTER_BOUND ( 'NONE', #13688, .T. ) ;
#11823 = DIRECTION ( 'NONE',  ( 0.000000000000000000, 0.000000000000000000, 1.000000000000000000 ) ) ;
#11824 = CIRCLE ( 'NONE', #12686, 2.500000000000000444 ) ;
#11825 = ORIENTED_EDGE ( 'NONE', *, *, #14310, .T. ) ;
#11826 =( LENGTH_UNIT ( ) NAMED_UNIT ( * ) SI_UNIT ( .MILLI., .METRE. ) );
#11828 = DIRECTION ( 'NONE',  ( 0.000000000000000000, 0.000000000000000000, 1.000000000000000000 ) ) ;
#11827 = AXIS2_PLACEMENT_3D ( 'NONE', #16971, #4839, #16717 ) ;
#11829 = ORIENTED_EDGE ( 'NONE', *, *, #15298, .F. ) ;
#11830 = PRODUCT_CONTEXT ( 'NONE', #4939, 'mechanical' ) ;
#11831 = CARTESIAN_POINT ( 'NONE',  ( -83.64137593015411198, 143.1840127716920676, 16.74578779913499460 ) ) ;
#11832 = CARTESIAN_POINT ( 'NONE',  ( 49.99999999999998579, 171.6227766016838245, 15.00000337241049131 ) ) ;
#11833 = CARTESIAN_POINT ( 'NONE',  ( -43.00000000000000000, 140.0000000000000000, 15.00000000000000000 ) ) ;
#11834 = VECTOR ( 'NONE', #7672, 1000.000000000000000 ) ;
#11835 = DIRECTION ( 'NONE',  ( 0.9961946980917464334, -0.04357787137382345549, -0.07547908730516519893 ) ) ;
#11836 = ORIENTED_EDGE ( 'NONE', *, *, #13166, .T. ) ;
#11837 = CARTESIAN_POINT ( 'NONE',  ( -73.00000000000001421, 171.6227766016838245, 0.000000000000000000 ) ) ;
#11838 = CIRCLE ( 'NONE', #12421, 5.000000000000004441 ) ;
#11839 = CARTESIAN_POINT ( 'NONE',  ( 50.00000000000000000, 146.6227766016838245, 0.000000000000000000 ) ) ;
#11840 = APPLICATION_CONTEXT ( 'automotive_design' ) ;
#11841 = EDGE_CURVE ( 'NONE', #13780, #13530, #8363, .T. ) ;
#11842 = CARTESIAN_POINT ( 'NONE',  ( -95.00000000000000000, 171.6227766016838245, 0.000000000000000000 ) ) ;
#11843 = CIRCLE ( 'NONE', #3654, 19.49999999999998934 ) ;
#11844 = CYLINDRICAL_SURFACE ( 'NONE', #6355, 27.69059892324149530 ) ;
#11845 = ORIENTED_EDGE ( 'NONE', *, *, #15009, .T. ) ;
#11846 = VERTEX_POINT ( 'NONE', #8544 ) ;
#11847 = CARTESIAN_POINT ( 'NONE',  ( 6.134011831684059501, 142.5209969267753820, -19.44444444444444642 ) ) ;
#11848 = VERTEX_POINT ( 'NONE', #318 ) ;
#11849 = LINE ( 'NONE', #11758, #5283 ) ;
#11850 = CARTESIAN_POINT ( 'NONE',  ( 11.37136921290580460, 130.9041960856249318, -11.49611652308843901 ) ) ;
#11851 = AXIS2_PLACEMENT_3D ( 'NONE', #10234, #4918, #7486 ) ;
#11852 = ORIENTED_EDGE ( 'NONE', *, *, #2329, .T. ) ;
#11853 = CARTESIAN_POINT ( 'NONE',  ( -151.0000000000000284, 171.6227766016838245, 23.57392898041429774 ) ) ;
#11854 = DIRECTION ( 'NONE',  ( 0.000000000000000000, 0.000000000000000000, 1.000000000000000000 ) ) ;
#11855 = CIRCLE ( 'NONE', #2546, 20.00000000000000355 ) ;
#11856 = CARTESIAN_POINT ( 'NONE',  ( 24.10793207926302983, 201.2861523353439566, -14.48313018527311868 ) ) ;
#11857 = CARTESIAN_POINT ( 'NONE',  ( 33.41144845724742396, 192.9634543217044609, 25.17141653689332870 ) ) ;
#11858 = DIRECTION ( 'NONE',  ( -1.000000000000000000, -0.000000000000000000, -0.000000000000000000 ) ) ;
#11859 = CARTESIAN_POINT ( 'NONE',  ( 23.09107716886297013, 17.99999999998395239, -5.538990817933217237 ) ) ;
#11860 = CARTESIAN_POINT ( 'NONE',  ( -14.99999999999999467, 90.00000000000000000, 15.00000000000000000 ) ) ;
#11861 = CARTESIAN_POINT ( 'NONE',  ( -206.1506185320109239, 215.7475848333072861, -31.15513424541605048 ) ) ;
#11862 = ADVANCED_FACE ( 'NONE', ( #5720, #5798 ), #11109, .T. ) ;
#11863 = EDGE_CURVE ( 'NONE', #8522, #8669, #8459, .T. ) ;
#11864 = CARTESIAN_POINT ( 'NONE',  ( 48.00000000000000711, 179.6227766016838245, -10.00000337241049309 ) ) ;
#11865 = EDGE_CURVE ( 'NONE', #12308, #6571, #11746, .T. ) ;
#11866 = CARTESIAN_POINT ( 'NONE',  ( 32.60692063061733137, 141.2146784997055988, -17.33162689407163981 ) ) ;
#11867 = VERTEX_POINT ( 'NONE', #3151 ) ;
#11868 = CARTESIAN_POINT ( 'NONE',  ( -38.00000000000000000, 18.00000000000000355, 0.000000000000000000 ) ) ;
#11869 = TOROIDAL_SURFACE ( 'NONE', #14149, 40.99999999999998579, 1.000000000000000000 ) ;
#11870 = CIRCLE ( 'NONE', #4803, 2.500000000000000444 ) ;
#11871 = ORIENTED_EDGE ( 'NONE', *, *, #394, .T. ) ;
#11872 = DIRECTION ( 'NONE',  ( -0.000000000000000000, -0.000000000000000000, -1.000000000000000000 ) ) ;
#11873 = VECTOR ( 'NONE', #15567, 1000.000000000000000 ) ;
#11874 = CARTESIAN_POINT ( 'NONE',  ( -12.63167751028164965, 18.00000000000000000, -24.35243221814330994 ) ) ;
#11875 = VERTEX_POINT ( 'NONE', #14924 ) ;
#11876 = CARTESIAN_POINT ( 'NONE',  ( -45.00000000000000711, -20.00000000000000000, -35.00000000000000000 ) ) ;
#11877 = CARTESIAN_POINT ( 'NONE',  ( 14.24852413927196970, 138.7494242586804489, 7.288003809479805639 ) ) ;
#11878 = VERTEX_POINT ( 'NONE', #13610 ) ;
#11879 = DIRECTION ( 'NONE',  ( 0.000000000000000000, 1.000000000000000000, 0.000000000000000000 ) ) ;
#11880 = ORIENTED_EDGE ( 'NONE', *, *, #8773, .T. ) ;
#11881 = AXIS2_PLACEMENT_3D ( 'NONE', #8089, #4115, #10837 ) ;
#11882 = CARTESIAN_POINT ( 'NONE',  ( 17.00000000000000000, 171.6227766016838245, 0.000000000000000000 ) ) ;
#11883 = DIRECTION ( 'NONE',  ( -1.000000000000000000, 0.000000000000000000, 0.000000000000000000 ) ) ;
#11884 = CARTESIAN_POINT ( 'NONE',  ( -23.00000000000000000, 120.0000000000000284, -4.999999999999999112 ) ) ;
#11885 = CARTESIAN_POINT ( 'NONE',  ( -22.80699178664539772, 18.00000000000000000, -18.33022619056923119 ) ) ;
#11886 = ORIENTED_EDGE ( 'NONE', *, *, #11403, .T. ) ;
#11887 = CARTESIAN_POINT ( 'NONE',  ( -206.3689767832464668, 123.5732568625972334, -24.35733450943962453 ) ) ;
#11888 = EDGE_LOOP ( 'NONE', ( #6800, #4677 ) ) ;
#11889 = CARTESIAN_POINT ( 'NONE',  ( 24.22171959708801481, 194.9977432358044780, -26.05112671349591125 ) ) ;
#11890 = CARTESIAN_POINT ( 'NONE',  ( -85.89206792073701990, 201.2861523353439281, -14.48313018527312046 ) ) ;
#11891 = CIRCLE ( 'NONE', #7944, 19.01029467089431080 ) ;
#11892 = ORIENTED_EDGE ( 'NONE', *, *, #8958, .F. ) ;
#11893 = EDGE_LOOP ( 'NONE', ( #1527, #13994, #339, #7541, #7135 ) ) ;
#11894 = VERTEX_POINT ( 'NONE', #1815 ) ;
#11895 = DIRECTION ( 'NONE',  ( -1.000000000000000000, 0.000000000000000000, 0.000000000000000000 ) ) ;
#11896 = ORIENTED_EDGE ( 'NONE', *, *, #4593, .F. ) ;
#11897 = DIRECTION ( 'NONE',  ( 1.000000000000000000, 0.000000000000000000, 0.000000000000000000 ) ) ;
#11898 = EDGE_CURVE ( 'NONE', #9311, #12797, #1588, .T. ) ;
#11899 = CARTESIAN_POINT ( 'NONE',  ( -7.379000772445021283, 30.00000000000000000, 13.00000000000000000 ) ) ;
#11900 = EDGE_CURVE ( 'NONE', #13709, #12308, #10634, .T. ) ;
#11901 = CARTESIAN_POINT ( 'NONE',  ( -13.49179905494335507, 31.33781166378165395, 13.29076615231557490 ) ) ;
#11902 = EDGE_CURVE ( 'NONE', #16058, #3793, #4133, .T. ) ;
#11903 = CARTESIAN_POINT ( 'NONE',  ( 27.00066514940125018, 151.8237148210351108, -28.86201951371925034 ) ) ;
#11904 = AXIS2_PLACEMENT_3D ( 'NONE', #17493, #5452, #4212 ) ;
#11905 = CARTESIAN_POINT ( 'NONE',  ( 20.77386775082738879, 29.88392224133981401, 10.47448535043027462 ) ) ;
#11906 = LINE ( 'NONE', #7571, #6089 ) ;
#11907 = VERTEX_POINT ( 'NONE', #6061 ) ;
#11908 = LINE ( 'NONE', #6516, #8420 ) ;
#11909 = CARTESIAN_POINT ( 'NONE',  ( 0.000000000000000000, 0.000000000000000000, 0.000000000000000000 ) ) ;
#11910 = CARTESIAN_POINT ( 'NONE',  ( 12.80996511848405994, 130.8496636614418094, 12.93682947221565804 ) ) ;
#11911 = DIRECTION ( 'NONE',  ( -1.000000000000000000, 0.000000000000000000, 0.000000000000000000 ) ) ;
#11912 = CARTESIAN_POINT ( 'NONE',  ( 22.45772829400591419, 29.90035839190693778, 11.59610751512981253 ) ) ;
#11913 = EDGE_LOOP ( 'NONE', ( #10280, #2946, #16242 ) ) ;
#11914 = LINE ( 'NONE', #13424, #7237 ) ;
#11915 = EDGE_CURVE ( 'NONE', #15739, #11936, #8878, .T. ) ;
#11916 = EDGE_CURVE ( 'NONE', #4396, #11681, #5833, .T. ) ;
#11917 = VERTEX_POINT ( 'NONE', #3577 ) ;
#11918 = CARTESIAN_POINT ( 'NONE',  ( -32.59761674097722306, 100.6207349242431093, -5.080178642862613003 ) ) ;
#11919 = DIRECTION ( 'NONE',  ( 0.000000000000000000, 0.000000000000000000, 1.000000000000000000 ) ) ;
#11920 = EDGE_LOOP ( 'NONE', ( #12267, #1936, #3272, #14542, #186, #382, #14409 ) ) ;
#11921 =( LENGTH_UNIT ( ) NAMED_UNIT ( * ) SI_UNIT ( .MILLI., .METRE. ) );
#11922 = CARTESIAN_POINT ( 'NONE',  ( -76.57381835343541354, 142.9679699711795990, 16.37278862731308493 ) ) ;
#11923 = EDGE_CURVE ( 'NONE', #4046, #4814, #17424, .T. ) ;
#11924 = CARTESIAN_POINT ( 'NONE',  ( 19.14963388379466736, 18.00000000000000000, -24.55317681541934149 ) ) ;
#11925 = DIRECTION ( 'NONE',  ( 0.000000000000000000, 0.4999999999999996669, 0.8660254037844388186 ) ) ;
#11926 = DIRECTION ( 'NONE',  ( 2.312964634635742464E-16, 0.000000000000000000, 1.000000000000000000 ) ) ;
#11927 = VERTEX_POINT ( 'NONE', #12710 ) ;
#11928 = DIRECTION ( 'NONE',  ( 0.000000000000000000, 0.000000000000000000, 1.000000000000000000 ) ) ;
#11929 = EDGE_CURVE ( 'NONE', #11970, #8095, #1999, .T. ) ;
#11930 = CARTESIAN_POINT ( 'NONE',  ( -50.00000000000000711, -20.00000000000000000, -35.00000000000000000 ) ) ;
#11931 = DIRECTION ( 'NONE',  ( 8.673617379884037937E-17, 0.000000000000000000, -1.000000000000000000 ) ) ;
#11932 = UNCERTAINTY_MEASURE_WITH_UNIT (LENGTH_MEASURE( 1.000000000000000082E-05 ), #16549, 'distance_accuracy_value', 'NONE');
#11933 = EDGE_CURVE ( 'NONE', #11959, #15924, #2158, .T. ) ;
#11934 = CARTESIAN_POINT ( 'NONE',  ( 35.83620472812211943, 198.0598900292994529, -22.94241666008127822 ) ) ;
#11935 = EDGE_CURVE ( 'NONE', #16184, #14270, #3000, .T. ) ;
#11936 = VERTEX_POINT ( 'NONE', #7467 ) ;
#11937 = ORIENTED_EDGE ( 'NONE', *, *, #687, .F. ) ;
#11938 = DIRECTION ( 'NONE',  ( 1.000000000000000000, 0.000000000000000000, -2.312964634635742957E-16 ) ) ;
#11939 = EDGE_LOOP ( 'NONE', ( #10258, #13644, #13397, #9587 ) ) ;
#11940 = CARTESIAN_POINT ( 'NONE',  ( -78.22656196874415002, 152.3723237521624014, -29.23070922465766941 ) ) ;
#11941 = CARTESIAN_POINT ( 'NONE',  ( 18.85693063297101801, 142.3798671548016159, -15.29581099734062022 ) ) ;
#11942 = EDGE_LOOP ( 'NONE', ( #9649, #7928 ) ) ;
#11943 = EDGE_CURVE ( 'NONE', #14947, #8170, #11457, .T. ) ;
#11944 = DIRECTION ( 'NONE',  ( -1.000000000000000000, 0.000000000000000000, 0.000000000000000000 ) ) ;
#11945 = CARTESIAN_POINT ( 'NONE',  ( -39.99999999999997158, 5.659323622547703371E-16, -33.00000000000000711 ) ) ;
#11946 = CARTESIAN_POINT ( 'NONE',  ( 22.50000000000000000, 196.6227766016838245, -21.54065922853802562 ) ) ;
#11947 =( REPRESENTATION_RELATIONSHIP ('NONE','NONE', #9723, #5345 ) REPRESENTATION_RELATIONSHIP_WITH_TRANSFORMATION ( #469 )SHAPE_REPRESENTATION_RELATIONSHIP( ) );
#11948 = CARTESIAN_POINT ( 'NONE',  ( -77.50000000000002842, 146.6227766016838245, 10.00000000000000178 ) ) ;
#11949 = DIRECTION ( 'NONE',  ( 0.000000000000000000, -0.000000000000000000, -1.000000000000000000 ) ) ;
#11950 = DIRECTION ( 'NONE',  ( 0.000000000000000000, -0.4999999999999997224, 0.8660254037844387076 ) ) ;
#11951 = FACE_OUTER_BOUND ( 'NONE', #13377, .T. ) ;
#11952 = CYLINDRICAL_SURFACE ( 'NONE', #8167, 7.500000000000007105 ) ;
#11953 = FACE_OUTER_BOUND ( 'NONE', #15539, .T. ) ;
#11954 = B_SPLINE_CURVE_WITH_KNOTS ( 'NONE', 3,
 ( #12942, #4879, #10268, #4961, #12850, #6471, #2392, #10355, #2051, #13198, #7786, #11866, #11518, #4800, #15671, #17274, #14355, #2221, #7617, #8784, #727, #16928, #13032, #902, #6289, #6564, #1430, #5416, #1340, #93, #4170, #8147, #14614, #7975, #12140, #13376, #1507, #9464, #3815, #2754, #6831, #14792 ),
 .UNSPECIFIED., .F., .F.,
 ( 4, 2, 2, 2, 2, 2, 2, 2, 2, 2, 2, 2, 2, 2, 2, 2, 2, 2, 2, 2, 4 ),
 ( 0.000000000000000000, 0.003174452718035283925, 0.004761679077052946921, 0.006348905436070610350, 0.007936131795088273780, 0.009523358154105937209, 0.01031697133361475678, 0.01111058451312357809, 0.01190419769263239939, 0.01230100428238680571, 0.01269781087214121203, 0.01349142405165002466, 0.01428503723115883729, 0.01507865041066764993, 0.01587226359017646082, 0.01745948994919411384, 0.01904671630821176340, 0.02063394266722941295, 0.02222116902624706250, 0.02380839538526471552, 0.02539562174428236160 ),
 .UNSPECIFIED. ) ;
#11955 = FACE_OUTER_BOUND ( 'NONE', #4651, .T. ) ;
#11956 = ORIENTED_EDGE ( 'NONE', *, *, #17330, .T. ) ;
#11957 = CARTESIAN_POINT ( 'NONE',  ( -5.000000000000000888, 154.3022685259950038, 9.999999999999900524 ) ) ;
#11958 = DIRECTION ( 'NONE',  ( 0.000000000000000000, 0.000000000000000000, -1.000000000000000000 ) ) ;
#11959 = VERTEX_POINT ( 'NONE', #14132 ) ;
#11960 = DIRECTION ( 'NONE',  ( 0.000000000000000000, 0.000000000000000000, 1.000000000000000000 ) ) ;
#11961 = CARTESIAN_POINT ( 'NONE',  ( -10.03891356649073785, 18.00000000000000355, -24.87483525495233394 ) ) ;
#11962 = ORIENTED_EDGE ( 'NONE', *, *, #11943, .F. ) ;
#11963 = CARTESIAN_POINT ( 'NONE',  ( 17.00000000000000000, 204.6227766016838245, 2.020667218593133100E-15 ) ) ;
#11964 = CARTESIAN_POINT ( 'NONE',  ( 12.95626684960129893, 129.1819364320672321, 10.30967895453046879 ) ) ;
#11965 = EDGE_CURVE ( 'NONE', #7127, #10963, #17124, .T. ) ;
#11966 = EDGE_LOOP ( 'NONE', ( #8602, #12452 ) ) ;
#11967 = ADVANCED_FACE ( 'NONE', ( #16868 ), #754, .F. ) ;
#11968 = CARTESIAN_POINT ( 'NONE',  ( 17.52239125723112778, 29.96525225773407186, 14.66037399604394942 ) ) ;
#11969 = ADVANCED_FACE ( 'NONE', ( #4739, #5985 ), #8628, .F. ) ;
#11970 = VERTEX_POINT ( 'NONE', #11631 ) ;
#11971 = DIRECTION ( 'NONE',  ( -1.000000000000000000, -0.000000000000000000, -0.000000000000000000 ) ) ;
#11972 = LINE ( 'NONE', #2324, #1959 ) ;
#11973 = LINE ( 'NONE', #9573, #15311 ) ;
#11974 = CARTESIAN_POINT ( 'NONE',  ( -10.04118010627651181, 18.00000000000000000, -24.87462214922868142 ) ) ;
#11975 = ORIENTED_EDGE ( 'NONE', *, *, #16163, .F. ) ;
#11976 = CARTESIAN_POINT ( 'NONE',  ( 31.34525843090159825, 151.4423111973152061, 26.11038153352143709 ) ) ;
#11977 = ORIENTED_EDGE ( 'NONE', *, *, #3171, .T. ) ;
#11978 = CARTESIAN_POINT ( 'NONE',  ( -85.08563460989527982, 191.1044234702846722, -26.63673872167001377 ) ) ;
#11979 = CARTESIAN_POINT ( 'NONE',  ( -208.0000000000000853, 174.7326106162513497, 0.000000000000000000 ) ) ;
#11980 = ORIENTED_EDGE ( 'NONE', *, *, #10337, .T. ) ;
#11981 = ORIENTED_EDGE ( 'NONE', *, *, #11929, .T. ) ;
#11982 = EDGE_LOOP ( 'NONE', ( #14671, #3675, #8064, #15909 ) ) ;
#11983 = CIRCLE ( 'NONE', #4354, 25.69059892324149175 ) ;
#11984 = ADVANCED_FACE ( 'NONE', ( #1907, #7398, #11288, #10131, #15356, #7304, #8725, #15536, #2249, #11546, #4650, #15618, #3493, #3328 ), #16702, .T. ) ;
#11985 = CARTESIAN_POINT ( 'NONE',  ( -80.56347832044305335, 154.1240291517870276, -27.97845313684488033 ) ) ;
#11986 = VERTEX_POINT ( 'NONE', #3845 ) ;
#11987 = DIRECTION ( 'NONE',  ( 0.000000000000000000, 0.000000000000000000, 1.000000000000000000 ) ) ;
#11988 = CARTESIAN_POINT ( 'NONE',  ( 13.65319468153969318, 138.6827642935804192, -2.302653601785663362 ) ) ;
#11989 = DIRECTION ( 'NONE',  ( 1.000000000000000000, 0.000000000000000000, 0.000000000000000000 ) ) ;
#11990 = CARTESIAN_POINT ( 'NONE',  ( 35.55667557412272828, 148.9132954376224802, -26.63594553516329455 ) ) ;
#11991 = DIRECTION ( 'NONE',  ( 0.000000000000000000, 0.000000000000000000, 1.000000000000000000 ) ) ;
#11992 = CARTESIAN_POINT ( 'NONE',  ( -78.47054368925184065, 151.3869516943736073, 26.06757126999134044 ) ) ;
#11993 = AXIS2_PLACEMENT_3D ( 'NONE', #12445, #4219, #16258 ) ;
#11994 = CIRCLE ( 'NONE', #4915, 5.000000000000007994 ) ;
#11995 = VERTEX_POINT ( 'NONE', #16062 ) ;
#11996 = CARTESIAN_POINT ( 'NONE',  ( -78.21870694796302814, 202.3573166656175317, -16.74530232247013828 ) ) ;
#11997 = LINE ( 'NONE', #3867, #832 ) ;
#11999 = CARTESIAN_POINT ( 'NONE',  ( -71.66708739526794147, 110.0000000000000142, 5.500000000000000000 ) ) ;
#11998 = CIRCLE ( 'NONE', #6634, 2.000000000000001776 ) ;
#12000 = FACE_OUTER_BOUND ( 'NONE', #12162, .T. ) ;
#12001 = CARTESIAN_POINT ( 'NONE',  ( 22.23780067492955936, 29.90321370453013117, 11.83858959072850858 ) ) ;
#12002 = EDGE_LOOP ( 'NONE', ( #7713, #8128 ) ) ;
#12003 = CARTESIAN_POINT ( 'NONE',  ( 39.99999999999999289, 8.000000000000000000, -39.99999999999999289 ) ) ;
#12004 = EDGE_CURVE ( 'NONE', #10173, #17455, #6961, .T. ) ;
#12005 = DIRECTION ( 'NONE',  ( -1.000000000000000000, -0.000000000000000000, 0.000000000000000000 ) ) ;
#12006 = DIRECTION ( 'NONE',  ( 0.8571673013836867971, 1.049727191973306626E-16, -0.5150380737757237481 ) ) ;
#12007 = ORIENTED_EDGE ( 'NONE', *, *, #77, .F. ) ;
#12008 = LINE ( 'NONE', #13257, #5863 ) ;
#12009 = DIRECTION ( 'NONE',  ( 0.000000000000000000, -1.000000000000000000, 0.000000000000000000 ) ) ;
#12010 = CIRCLE ( 'NONE', #2387, 19.49999999999998934 ) ;
#12011 = ORIENTED_EDGE ( 'NONE', *, *, #8739, .T. ) ;
#12012 = CARTESIAN_POINT ( 'NONE',  ( -75.79427778309866426, 143.8556217771935053, 17.85322440072383898 ) ) ;
#12013 = CARTESIAN_POINT ( 'NONE',  ( -102.0000000000000142, 171.6227766016838245, -25.69059892324149175 ) ) ;
#12014 = CARTESIAN_POINT ( 'NONE',  ( -75.92798022420988957, 142.2001748967346941, -18.96071578072434249 ) ) ;
#12015 = CARTESIAN_POINT ( 'NONE',  ( -17.58288004918492931, 20.00000000000000355, 22.43027208364174285 ) ) ;
#12016 = ORIENTED_EDGE ( 'NONE', *, *, #8483, .T. ) ;
#12017 = CARTESIAN_POINT ( 'NONE',  ( 49.99999999999998579, 183.6227766016837961, -8.071800142134975431 ) ) ;
#12018 = CARTESIAN_POINT ( 'NONE',  ( 9.156206820864191798, 144.1010407228830559, 18.21082046960973599 ) ) ;
#12019 = DIRECTION ( 'NONE',  ( 0.000000000000000000, 0.000000000000000000, 1.000000000000000000 ) ) ;
#12020 = DIRECTION ( 'NONE',  ( 0.000000000000000000, 0.000000000000000000, 1.000000000000000000 ) ) ;
#12021 = VECTOR ( 'NONE', #5049, 1000.000000000000000 ) ;
#12022 = VECTOR ( 'NONE', #6188, 1000.000000000000000 ) ;
#12023 = EDGE_CURVE ( 'NONE', #12513, #9911, #16291, .T. ) ;
#12024 = AXIS2_PLACEMENT_3D ( 'NONE', #7230, #15101, #7061 ) ;
#12025 = VERTEX_POINT ( 'NONE', #2690 ) ;
#12026 = TOROIDAL_SURFACE ( 'NONE', #14291, 25.00000000000000000, 8.000000000000000000 ) ;
#12027 = PLANE ( 'NONE',  #1339 ) ;
#12028 = ORIENTED_EDGE ( 'NONE', *, *, #12113, .T. ) ;
#12029 = CARTESIAN_POINT ( 'NONE',  ( -80.47498095768615656, 152.6213468612616566, -29.39295273708632550 ) ) ;
#12030 = CARTESIAN_POINT ( 'NONE',  ( 14.40174056114590151, 138.5906827818587885, -4.212836247846349025 ) ) ;
#12031 = ORIENTED_EDGE ( 'NONE', *, *, #13705, .F. ) ;
#12032 = CARTESIAN_POINT ( 'NONE',  ( -27.99999999999998224, 10.00000000000000000, 10.00000000000000178 ) ) ;
#12033 = CARTESIAN_POINT ( 'NONE',  ( -31.89848094669886436, 119.9728602285818084, -5.500000000000000000 ) ) ;
#12034 = EDGE_CURVE ( 'NONE', #13477, #2095, #9490, .T. ) ;
#12035 = EDGE_CURVE ( 'NONE', #12970, #1757, #1097, .T. ) ;
#12036 = AXIS2_PLACEMENT_3D ( 'NONE', #2723, #67, #5554 ) ;
#12037 = DIRECTION ( 'NONE',  ( 0.000000000000000000, 0.000000000000000000, 1.000000000000000000 ) ) ;
#12038 = AXIS2_PLACEMENT_3D ( 'NONE', #8825, #2181, #16803 ) ;
#12039 = CARTESIAN_POINT ( 'NONE',  ( -30.49999999999998224, 10.00000000000000000, 0.000000000000000000 ) ) ;
#12040 = DIRECTION ( 'NONE',  ( 0.000000000000000000, 0.000000000000000000, -1.000000000000000000 ) ) ;
#12041 = CARTESIAN_POINT ( 'NONE',  ( 31.20232444244219394, 18.00000000000000000, -16.65183244245019623 ) ) ;
#12042 = DIRECTION ( 'NONE',  ( 1.000000000000000000, -0.000000000000000000, -0.000000000000000000 ) ) ;
#12043 = CARTESIAN_POINT ( 'NONE',  ( -95.00000000000000000, 201.6227766016838245, -1.836970198721029589E-15 ) ) ;
#12044 = CARTESIAN_POINT ( 'NONE',  ( 0.000000000000000000, 0.000000000000000000, 0.000000000000000000 ) ) ;
#12045 = ORIENTED_EDGE ( 'NONE', *, *, #12411, .T. ) ;
#12046 = CARTESIAN_POINT ( 'NONE',  ( -45.00000000000000000, 122.0000000000000142, 0.000000000000000000 ) ) ;
#12047 = ORIENTED_EDGE ( 'NONE', *, *, #1362, .T. ) ;
#12048 = DIRECTION ( 'NONE',  ( 0.000000000000000000, 0.000000000000000000, 1.000000000000000000 ) ) ;
#12049 = CLOSED_SHELL ( 'NONE', ( #11551, #9586, #12134, #1899, #9650, #14884 ) ) ;
#12050 = AXIS2_PLACEMENT_3D ( 'NONE', #12255, #129, #5530 ) ;
#12051 = CARTESIAN_POINT ( 'NONE',  ( -43.00000000000000000, 140.0000000000000000, 13.00000000000000000 ) ) ;
#12052 = AXIS2_PLACEMENT_3D ( 'NONE', #7049, #6873, #5542 ) ;
#12053 = ORIENTED_EDGE ( 'NONE', *, *, #8845, .T. ) ;
#12054 = CARTESIAN_POINT ( 'NONE',  ( -10.00647404944701258, 20.00000000000000000, 14.03129316391565951 ) ) ;
#12055 = CARTESIAN_POINT ( 'NONE',  ( 26.76721132277178228, 139.3994271089711958, 7.121518580654788266 ) ) ;
#12056 = ORIENTED_EDGE ( 'NONE', *, *, #10444, .F. ) ;
#12057 = DIRECTION ( 'NONE',  ( -0.8660254037844378194, -0.5000000000000015543, -0.000000000000000000 ) ) ;
#12058 = EDGE_LOOP ( 'NONE', ( #14551, #12773 ) ) ;
#12059 = DIRECTION ( 'NONE',  ( 0.000000000000000000, -1.000000000000000000, 1.836970198721028701E-16 ) ) ;
#12060 = CIRCLE ( 'NONE', #8378, 24.99999999999999645 ) ;
#12061 = AXIS2_PLACEMENT_3D ( 'NONE', #11766, #8851, #10187 ) ;
#12062 = CARTESIAN_POINT ( 'NONE',  ( -208.1243352336974510, 176.1537688404888513, 3.744334046054181186 ) ) ;
#12063 = CARTESIAN_POINT ( 'NONE',  ( 48.00000000000000711, 159.6227766016838814, -5.571800142134975431 ) ) ;
#12064 = AXIS2_PLACEMENT_3D ( 'NONE', #8355, #16778, #4643 ) ;
#12065 = CARTESIAN_POINT ( 'NONE',  ( 49.99999999999998579, 163.6227766016838530, 12.50000337241049309 ) ) ;
#12066 = VECTOR ( 'NONE', #9918, 1000.000000000000000 ) ;
#12067 = ORIENTED_EDGE ( 'NONE', *, *, #13974, .F. ) ;
#12068 = CARTESIAN_POINT ( 'NONE',  ( 25.07772090985335467, 147.6670862717896000, 22.70911985051488458 ) ) ;
#12069 = EDGE_CURVE ( 'NONE', #5481, #4609, #168, .T. ) ;
#12070 = EDGE_LOOP ( 'NONE', ( #9877, #13223, #9351 ) ) ;
#12071 = DIRECTION ( 'NONE',  ( 2.312964634635742464E-16, 0.000000000000000000, -1.000000000000000000 ) ) ;
#12072 = PLANE ( 'NONE',  #8657 ) ;
#12073 = ORIENTED_EDGE ( 'NONE', *, *, #2212, .F. ) ;
#12074 = ORIENTED_EDGE ( 'NONE', *, *, #1993, .T. ) ;
#12075 = VERTEX_POINT ( 'NONE', #13057 ) ;
#12076 = CIRCLE ( 'NONE', #16612, 20.00000000000000355 ) ;
#12077 = VECTOR ( 'NONE', #14170, 1000.000000000000000 ) ;
#12079 = CARTESIAN_POINT ( 'NONE',  ( 6.851232759387628768, 134.0993825829163200, 14.99999999999999822 ) ) ;
#12078 =( GEOMETRIC_REPRESENTATION_CONTEXT ( 3 ) GLOBAL_UNCERTAINTY_ASSIGNED_CONTEXT ( ( #8775 ) ) GLOBAL_UNIT_ASSIGNED_CONTEXT ( ( #148, #2974, #8284 ) ) REPRESENTATION_CONTEXT ( 'NONE', 'WORKASPACE' ) );
#12080 = VECTOR ( 'NONE', #324, 1000.000000000000000 ) ;
#12081 = ORIENTED_EDGE ( 'NONE', *, *, #2498, .F. ) ;
#12082 =( NAMED_UNIT ( * ) SI_UNIT ( $, .STERADIAN. ) SOLID_ANGLE_UNIT ( ) );
#12083 = DIRECTION ( 'NONE',  ( -1.000000000000000000, -0.000000000000000000, -0.000000000000000000 ) ) ;
#12084 = LINE ( 'NONE', #15170, #427 ) ;
#12085 = CARTESIAN_POINT ( 'NONE',  ( 29.07646442517566854, 152.5685199100059322, -29.35899209070759142 ) ) ;
#12086 = LINE ( 'NONE', #13509, #11627 ) ;
#12087 = CARTESIAN_POINT ( 'NONE',  ( -3.000000000000000888, 191.6227766016837961, -1.224646799147353454E-15 ) ) ;
#12088 = ORIENTED_EDGE ( 'NONE', *, *, #12828, .F. ) ;
#12089 = CARTESIAN_POINT ( 'NONE',  ( -34.99999999999999289, 120.0000000000000284, 4.999999999999999112 ) ) ;
#12090 = DIRECTION ( 'NONE',  ( 0.000000000000000000, 0.000000000000000000, -1.000000000000000000 ) ) ;
#12091 = EDGE_CURVE ( 'NONE', #10963, #7127, #2429, .T. ) ;
#12092 = EDGE_CURVE ( 'NONE', #8820, #13139, #9234, .T. ) ;
#12093 = VECTOR ( 'NONE', #7595, 1000.000000000000000 ) ;
#12094 = CARTESIAN_POINT ( 'NONE',  ( 17.54349574104648823, 125.4948194589026684, 4.999999999999997335 ) ) ;
#12095 = EDGE_CURVE ( 'NONE', #4421, #1696, #10555, .T. ) ;
#12096 = PRODUCT_DEFINITION_FORMATION_WITH_SPECIFIED_SOURCE ( 'ANY', '', #1494, .NOT_KNOWN. ) ;
#12097 = CARTESIAN_POINT ( 'NONE',  ( 34.93420767853316988, 18.00000000000000355, 4.999999999999999112 ) ) ;
#12098 = DIRECTION ( 'NONE',  ( -1.000000000000000000, 0.000000000000000000, 0.000000000000000000 ) ) ;
#12099 = ADVANCED_FACE ( 'NONE', ( #13225 ), #12072, .T. ) ;
#12100 = ORIENTED_EDGE ( 'NONE', *, *, #14886, .F. ) ;
#12101 = CARTESIAN_POINT ( 'NONE',  ( -22.99999999999999645, 100.0000000000000142, 15.00000000000000000 ) ) ;
#12102 = CIRCLE ( 'NONE', #7287, 9.999999999999998224 ) ;
#12103 = CARTESIAN_POINT ( 'NONE',  ( 6.134011831684053284, 134.2062027339443944, -25.00000000000000000 ) ) ;
#12104 = ORIENTED_EDGE ( 'NONE', *, *, #8940, .F. ) ;
#12105 = CARTESIAN_POINT ( 'NONE',  ( -90.80384757729339640, 171.6227766016838245, 0.000000000000000000 ) ) ;
#12106 = VERTEX_POINT ( 'NONE', #15791 ) ;
#12107 = CIRCLE ( 'NONE', #7850, 7.500000000000003553 ) ;
#12108 = CARTESIAN_POINT ( 'NONE',  ( 27.99999999999998224, 9.999999999999998224, -13.00000000000000000 ) ) ;
#12109 = AXIS2_PLACEMENT_3D ( 'NONE', #423, #9634, #4253 ) ;
#12110 = STYLED_ITEM ( 'NONE', ( #11486 ), #10572 ) ;
#12111 = CARTESIAN_POINT ( 'NONE',  ( -98.00000000000000000, 171.6227766016838245, 5.000000000000006217 ) ) ;
#12112 = CARTESIAN_POINT ( 'NONE',  ( -78.69116039514727845, 140.7623173628079485, -16.51208758287213030 ) ) ;
#12113 = EDGE_CURVE ( 'NONE', #15648, #3748, #15606, .T. ) ;
#12114 = CARTESIAN_POINT ( 'NONE',  ( -19.25702671965661850, 19.99999999999999645, 21.36300512502526416 ) ) ;
#12115 = ORIENTED_EDGE ( 'NONE', *, *, #7648, .F. ) ;
#12116 = FACE_OUTER_BOUND ( 'NONE', #2642, .T. ) ;
#12117 = CARTESIAN_POINT ( 'NONE',  ( 14.29542716350633214, 143.4273548044023698, 17.14909632368674508 ) ) ;
#12118 = CARTESIAN_POINT ( 'NONE',  ( 39.99999999999998579, 8.000000000000000000, -29.99999999999999645 ) ) ;
#12119 = CARTESIAN_POINT ( 'NONE',  ( 27.75000000000000000, 0.000000000000000000, 2.055000000000000160 ) ) ;
#12120 = VECTOR ( 'NONE', #13294, 1000.000000000000000 ) ;
#12121 = AXIS2_PLACEMENT_3D ( 'NONE', #1567, #5731, #13528 ) ;
#12122 = VERTEX_POINT ( 'NONE', #5079 ) ;
#12123 = CARTESIAN_POINT ( 'NONE',  ( 16.35719767791491819, 136.8501131444031387, -5.449348266248646766 ) ) ;
#12124 = ORIENTED_EDGE ( 'NONE', *, *, #7910, .F. ) ;
#12125 = CARTESIAN_POINT ( 'NONE',  ( -74.95697939493170736, 149.8947795965756029, -27.44208088385415323 ) ) ;
#12126 = CARTESIAN_POINT ( 'NONE',  ( 22.72753210816364700, 141.1551838527312555, -12.68377836492884470 ) ) ;
#12127 = VERTEX_POINT ( 'NONE', #7912 ) ;
#12128 = DIRECTION ( 'NONE',  ( -1.000000000000000000, 0.000000000000000000, 0.000000000000000000 ) ) ;
#12129 = PLANE ( 'NONE',  #2829 ) ;
#12130 = DIRECTION ( 'NONE',  ( 0.000000000000000000, 0.000000000000000000, 1.000000000000000000 ) ) ;
#12131 = ADVANCED_FACE ( 'NONE', ( #13320 ), #11480, .F. ) ;
#12132 = AXIS2_PLACEMENT_3D ( 'NONE', #13953, #7397, #7131 ) ;
#12133 = CARTESIAN_POINT ( 'NONE',  ( -80.00000000000002842, 146.6227766016838245, 1.387778780781445676E-14 ) ) ;
#12134 = ADVANCED_FACE ( 'NONE', ( #1184 ), #6589, .T. ) ;
#12135 = AXIS2_PLACEMENT_3D ( 'NONE', #11469, #8735, #598 ) ;
#12136 = CARTESIAN_POINT ( 'NONE',  ( 22.61491075001043782, 18.00000000000000000, -23.50024419593056635 ) ) ;
#12137 = CARTESIAN_POINT ( 'NONE',  ( 22.12396056536369215, 29.85772992373802026, -8.548742771607255264 ) ) ;
#12138 = CARTESIAN_POINT ( 'NONE',  ( 30.00000000000000355, 196.6227766016838245, -16.00000000000000000 ) ) ;
#12139 = LINE ( 'NONE', #1338, #12158 ) ;
#12140 = CARTESIAN_POINT ( 'NONE',  ( 25.01160876918508791, 143.2703805450037180, -20.52792728560773483 ) ) ;
#12141 = ORIENTED_EDGE ( 'NONE', *, *, #15281, .F. ) ;
#12142 = CARTESIAN_POINT ( 'NONE',  ( 6.134011831684053284, 134.2062027339443944, -15.00000000000000000 ) ) ;
#12143 = EDGE_LOOP ( 'NONE', ( #1274, #5585 ) ) ;
#12144 = CARTESIAN_POINT ( 'NONE',  ( -18.25212770525996930, 32.30769230769230660, 15.00000000000000000 ) ) ;
#12145 = EDGE_CURVE ( 'NONE', #4581, #13903, #13401, .T. ) ;
#12146 = CIRCLE ( 'NONE', #2816, 6.000000000000005329 ) ;
#12147 = CARTESIAN_POINT ( 'NONE',  ( 16.17028938446068764, 143.0439382767918346, -16.49999999999050360 ) ) ;
#12148 = VECTOR ( 'NONE', #6127, 1000.000000000000000 ) ;
#12149 = ORIENTED_EDGE ( 'NONE', *, *, #2314, .T. ) ;
#12150 = CARTESIAN_POINT ( 'NONE',  ( -19.26597175465490963, 19.99999999999999645, 21.35691006828317384 ) ) ;
#12151 = AXIS2_PLACEMENT_3D ( 'NONE', #9000, #14412, #5193 ) ;
#12152 = CARTESIAN_POINT ( 'NONE',  ( 14.50951369217283826, 138.6207054667691523, 6.378636156063609342 ) ) ;
#12153 = EDGE_LOOP ( 'NONE', ( #12246, #8762, #2968, #9991 ) ) ;
#12154 = CARTESIAN_POINT ( 'NONE',  ( -74.00000000000001421, 196.6227766016838245, -24.49489742783179125 ) ) ;
#12155 = VERTEX_POINT ( 'NONE', #16158 ) ;
#12156 = DIRECTION ( 'NONE',  ( -0.000000000000000000, -0.000000000000000000, -1.000000000000000000 ) ) ;
#12157 = CARTESIAN_POINT ( 'NONE',  ( 49.99999999999998579, 175.6227766016838245, -8.071800142134975431 ) ) ;
#12158 = VECTOR ( 'NONE', #2662, 1000.000000000000000 ) ;
#12159 = LINE ( 'NONE', #8163, #7668 ) ;
#12160 = CARTESIAN_POINT ( 'NONE',  ( -116.4755503550297107, 171.6227766016838245, 78.75916623668499028 ) ) ;
#12161 = VECTOR ( 'NONE', #14699, 1000.000000000000000 ) ;
#12162 = EDGE_LOOP ( 'NONE', ( #16561, #5238, #1846, #8564 ) ) ;
#12163 = CARTESIAN_POINT ( 'NONE',  ( 30.77905682277627619, 151.5769270156786206, 26.21405625665653005 ) ) ;
#12164 = EDGE_LOOP ( 'NONE', ( #9495, #3057, #1790, #14507, #3228, #16161 ) ) ;
#12165 = CARTESIAN_POINT ( 'NONE',  ( -34.99999999999999289, 120.0000000000000284, -15.00000000000000000 ) ) ;
#12166 = CARTESIAN_POINT ( 'NONE',  ( 25.00000000000000000, 196.6227766016838245, 0.000000000000000000 ) ) ;
#12167 = EDGE_CURVE ( 'NONE', #17455, #15648, #4033, .T. ) ;
#12168 = VERTEX_POINT ( 'NONE', #8079 ) ;
#12169 = VERTEX_POINT ( 'NONE', #13493 ) ;
#12170 = EDGE_LOOP ( 'NONE', ( #8000, #1858 ) ) ;
#12171 = AXIS2_PLACEMENT_3D ( 'NONE', #11313, #15472, #6005 ) ;
#12172 = AXIS2_PLACEMENT_3D ( 'NONE', #2269, #3432, #16886 ) ;
#12173 = B_SPLINE_CURVE_WITH_KNOTS ( 'NONE', 3,
 ( #7419, #2027, #4511, #9900, #8662, #7338, #5927, #16647, #12821, #6091, #15305, #8569, #14073, #11487, #12910, #786, #11576, #16896, #8752, #3260, #13981, #12999 ),
 .UNSPECIFIED., .F., .F.,
 ( 4, 2, 2, 2, 2, 2, 2, 2, 2, 2, 4 ),
 ( 0.000000000000000000, 0.003698315653799323904, 0.007396631307598647807, 0.01109494696139797128, 0.01479326261519729561, 0.01664242044209697166, 0.01849157826899665291, 0.02218989392279601541, 0.02403905174969570360, 0.02588820957659539179, 0.02958652523039474735 ),
 .UNSPECIFIED. ) ;
#12174 = CARTESIAN_POINT ( 'NONE',  ( 11.08062248138347528, 138.8595139650515193, 13.56485289974971842 ) ) ;
#12175 = AXIS2_PLACEMENT_3D ( 'NONE', #2975, #6710, #16268 ) ;
#12176 = ORIENTED_EDGE ( 'NONE', *, *, #10638, .F. ) ;
#12177 = APPLICATION_PROTOCOL_DEFINITION ( 'draft international standard', 'automotive_design', 1998, #11840 ) ;
#12178 = ADVANCED_FACE ( 'NONE', ( #4197 ), #6773, .F. ) ;
#12179 = DIRECTION ( 'NONE',  ( 0.000000000000000000, 0.000000000000000000, -1.000000000000000000 ) ) ;
#12180 = DIRECTION ( 'NONE',  ( -1.000000000000000000, 0.000000000000000000, 0.000000000000000000 ) ) ;
#12181 = CARTESIAN_POINT ( 'NONE',  ( -3.000000000000002665, 142.8100939375178200, 16.63501009223129756 ) ) ;
#12182 = CYLINDRICAL_SURFACE ( 'NONE', #11904, 33.00000000000000000 ) ;
#12183 = CARTESIAN_POINT ( 'NONE',  ( -83.01610148909772136, 150.6144458722573063, 25.44936967851740306 ) ) ;
#12184 = ORIENTED_EDGE ( 'NONE', *, *, #1031, .T. ) ;
#12185 = CARTESIAN_POINT ( 'NONE',  ( -80.25501005280430888, 202.6234830987601185, -16.24672887513765929 ) ) ;
#12186 = CIRCLE ( 'NONE', #4553, 740.0000000000000000 ) ;
#12187 = CARTESIAN_POINT ( 'NONE',  ( 17.51892952578853979, 125.6677330052578014, 5.783603459598163354 ) ) ;
#12188 = CARTESIAN_POINT ( 'NONE',  ( 29.54149365486396661, 18.00000000000000355, 18.67620474358521676 ) ) ;
#12189 = AXIS2_PLACEMENT_3D ( 'NONE', #16509, #9336, #2618 ) ;
#12190 = CARTESIAN_POINT ( 'NONE',  ( -206.6026792233873550, 173.6007525171767440, 4.555693436530018126 ) ) ;
#12191 = DIRECTION ( 'NONE',  ( -1.000000000000000000, 0.000000000000000000, 0.000000000000000000 ) ) ;
#12192 = DIRECTION ( 'NONE',  ( 1.000000000000000000, 0.000000000000000000, 0.000000000000000000 ) ) ;
#12193 = VERTEX_POINT ( 'NONE', #12166 ) ;
#12194 = AXIS2_PLACEMENT_3D ( 'NONE', #6600, #11991, #17396 ) ;
#12195 = ORIENTED_EDGE ( 'NONE', *, *, #16740, .F. ) ;
#12196 = EDGE_CURVE ( 'NONE', #12777, #10642, #6927, .T. ) ;
#12197 = EDGE_CURVE ( 'NONE', #313, #17135, #13750, .T. ) ;
#12198 = CARTESIAN_POINT ( 'NONE',  ( -68.00000000000000000, 143.0439382767972347, -16.49999999999984368 ) ) ;
#12199 = EDGE_CURVE ( 'NONE', #10626, #10459, #16007, .T. ) ;
#12200 = FACE_OUTER_BOUND ( 'NONE', #4600, .T. ) ;
#12201 = CARTESIAN_POINT ( 'NONE',  ( -207.6775903968323576, 166.3720764825075662, 1.150672365064113079 ) ) ;
#12202 = CARTESIAN_POINT ( 'NONE',  ( -27.94760966554430937, 19.99999999999999645, 6.338314452217975514 ) ) ;
#12203 = EDGE_LOOP ( 'NONE', ( #12406, #6591, #1360, #14687 ) ) ;
#12204 = CARTESIAN_POINT ( 'NONE',  ( 27.99999999999998224, 9.999999999999998224, 0.000000000000000000 ) ) ;
#12205 = DIRECTION ( 'NONE',  ( 1.000000000000000000, 0.000000000000000000, 0.000000000000000000 ) ) ;
#12206 = LINE ( 'NONE', #15025, #15556 ) ;
#12207 = DIRECTION ( 'NONE',  ( -1.000000000000000000, 0.000000000000000000, 0.000000000000000000 ) ) ;
#12208 = AXIS2_PLACEMENT_3D ( 'NONE', #9926, #16414, #16577 ) ;
#12209 = CARTESIAN_POINT ( 'NONE',  ( 24.34257225596279639, 138.6622241066778543, -11.80661878326775494 ) ) ;
#12210 = VERTEX_POINT ( 'NONE', #1456 ) ;
#12211 = DIRECTION ( 'NONE',  ( 8.673617379884037937E-17, 0.000000000000000000, 1.000000000000000000 ) ) ;
#12212 = CARTESIAN_POINT ( 'NONE',  ( 2.749999999999999112, 0.000000000000000000, 4.750000000000000000 ) ) ;
#12213 = ORIENTED_EDGE ( 'NONE', *, *, #12196, .T. ) ;
#12214 = DIRECTION ( 'NONE',  ( 0.000000000000000000, 0.000000000000000000, 1.000000000000000000 ) ) ;
#12215 = CYLINDRICAL_SURFACE ( 'NONE', #11531, 2.499999999999998668 ) ;
#12216 = CARTESIAN_POINT ( 'NONE',  ( 0.000000000000000000, 0.000000000000000000, 0.000000000000000000 ) ) ;
#12217 = CARTESIAN_POINT ( 'NONE',  ( 32.91012024024373517, 17.99999999999999645, -13.86436652238006673 ) ) ;
#12218 = CARTESIAN_POINT ( 'NONE',  ( 21.03896850327811663, 17.99999999999885247, -10.35865908471247643 ) ) ;
#12219 = LINE ( 'NONE', #349, #5010 ) ;
#12220 = FACE_OUTER_BOUND ( 'NONE', #11339, .T. ) ;
#12221 = FACE_BOUND ( 'NONE', #2368, .T. ) ;
#12222 = FACE_OUTER_BOUND ( 'NONE', #6363, .T. ) ;
#12223 = ORIENTED_EDGE ( 'NONE', *, *, #3538, .F. ) ;
#12224 = CARTESIAN_POINT ( 'NONE',  ( 11.67974368446408384, 131.7296502858855547, -13.62018484423547804 ) ) ;
#12225 = VERTEX_POINT ( 'NONE', #2863 ) ;
#12226 = CARTESIAN_POINT ( 'NONE',  ( 30.00000000000001066, 146.6227766016838245, -16.00000000000000000 ) ) ;
#12227 = FACE_OUTER_BOUND ( 'NONE', #6148, .T. ) ;
#12228 = ORIENTED_EDGE ( 'NONE', *, *, #11493, .T. ) ;
#12229 = EDGE_CURVE ( 'NONE', #15996, #3972, #9493, .T. ) ;
#12230 = CARTESIAN_POINT ( 'NONE',  ( -16.58710929330769090, 31.97525413706907216, 10.34574908881256050 ) ) ;
#12231 = CARTESIAN_POINT ( 'NONE',  ( -7.379000772444994638, 30.00000000000000000, 15.00000000000000000 ) ) ;
#12232 = EDGE_LOOP ( 'NONE', ( #12838, #14361, #9753 ) ) ;
#12233 = CARTESIAN_POINT ( 'NONE',  ( 35.08563460989521587, 152.1411297330830621, -26.63673872167000667 ) ) ;
#12234 = ORIENTED_EDGE ( 'NONE', *, *, #499, .T. ) ;
#12235 = CARTESIAN_POINT ( 'NONE',  ( -38.00000000000000000, 20.00000000000000000, -30.00000000000000355 ) ) ;
#12236 = DIRECTION ( 'NONE',  ( 0.000000000000000000, 0.000000000000000000, -1.000000000000000000 ) ) ;
#12237 = LINE ( 'NONE', #107, #11355 ) ;
#12238 = ORIENTED_EDGE ( 'NONE', *, *, #12535, .T. ) ;
#12239 = CARTESIAN_POINT ( 'NONE',  ( 34.99999999999999289, -20.00000000000000000, -35.00000000000002132 ) ) ;
#12240 = VERTEX_POINT ( 'NONE', #7024 ) ;
#12241 = CARTESIAN_POINT ( 'NONE',  ( 28.08965273233581073, 151.2585272520459512, 25.96811968750270339 ) ) ;
#12242 = ORIENTED_EDGE ( 'NONE', *, *, #5249, .F. ) ;
#12243 = CARTESIAN_POINT ( 'NONE',  ( -81.17267072074459122, 189.2094081997700528, -27.92332374485731350 ) ) ;
#12244 = CARTESIAN_POINT ( 'NONE',  ( -100.0000000000000000, 100.0000000000000142, 0.000000000000000000 ) ) ;
#12245 = CARTESIAN_POINT ( 'NONE',  ( -13.00560346926692645, 31.78932620563996281, -11.23370548922391521 ) ) ;
#12246 = ORIENTED_EDGE ( 'NONE', *, *, #13208, .F. ) ;
#12247 = ORIENTED_EDGE ( 'NONE', *, *, #4740, .T. ) ;
#12248 = ADVANCED_FACE ( 'NONE', ( #5697, #8258, #39 ), #14901, .T. ) ;
#12249 = CARTESIAN_POINT ( 'NONE',  ( 15.42236477930650906, 141.4984257577436892, 17.82510376534603580 ) ) ;
#12250 = EDGE_CURVE ( 'NONE', #2195, #13060, #205, .T. ) ;
#12251 = VERTEX_POINT ( 'NONE', #4286 ) ;
#12252 = SHAPE_DEFINITION_REPRESENTATION ( #13651, #16423 ) ;
#12253 = CARTESIAN_POINT ( 'NONE',  ( -45.00000000000001421, 124.1421356237309368, 15.00000000000000355 ) ) ;
#12254 = EDGE_CURVE ( 'NONE', #11543, #14137, #9667, .T. ) ;
#12255 = CARTESIAN_POINT ( 'NONE',  ( 27.99999999999998224, 9.999999999999998224, -35.00200000000000244 ) ) ;
#12256 = EDGE_CURVE ( 'NONE', #583, #2837, #2944, .T. ) ;
#12257 = B_SPLINE_CURVE_WITH_KNOTS ( 'NONE', 3,
 ( #16944, #4818, #10208, #655, #3405, #16776, #7201, #744, #14031, #3484, #10022, #15435, #3316, #8712, #11184, #476, #5880, #14277, #14120, #1987, #2148, #7388, #12785, #6052, #8798, #11446, #12521, #385, #16858, #14205, #8535, #2064, #7456, #12865, #16601, #4474, #9858, #15265, #3140, #13945 ),
 .UNSPECIFIED., .F., .F.,
 ( 4, 2, 2, 2, 2, 2, 2, 2, 2, 2, 2, 2, 2, 2, 2, 2, 2, 2, 2, 4 ),
 ( 0.02243093923957190788, 0.02359459467514175152, 0.02475825011071159515, 0.02592190554628143878, 0.02708556098185128241, 0.02766738869963622505, 0.02824921641742116421, 0.02941287185299101478, 0.03057652728856086188, 0.03115835500634581492, 0.03174018272413076797, 0.03232201044191572448, 0.03290383815970067405, 0.03348566587748562362, 0.03406749359527058013, 0.03523114903084052785, 0.03639480446641046862, 0.03755845990198040940, 0.03872211533755035018, 0.04104942620869018316 ),
 .UNSPECIFIED. ) ;
#12258 = CARTESIAN_POINT ( 'NONE',  ( 22.88339857903067198, 29.84310082762161187, -6.047897139192784266 ) ) ;
#12259 = DIRECTION ( 'NONE',  ( -0.000000000000000000, -0.000000000000000000, 1.000000000000000000 ) ) ;
#12260 = CARTESIAN_POINT ( 'NONE',  ( 0.000000000000000000, 20.00000000000000000, -25.00000000000000000 ) ) ;
#12261 = EDGE_LOOP ( 'NONE', ( #7498, #3135, #15070, #6236 ) ) ;
#12262 = CARTESIAN_POINT ( 'NONE',  ( -85.73889985627347698, 198.4077499201237060, -22.53509453904544557 ) ) ;
#12263 = CARTESIAN_POINT ( 'NONE',  ( -151.6393416600920716, 171.6227766016838245, -25.46898629924947244 ) ) ;
#12264 = CARTESIAN_POINT ( 'NONE',  ( 34.42405209918207731, 19.99999999999999289, -9.535225002503356251 ) ) ;
#12265 = CARTESIAN_POINT ( 'NONE',  ( -27.99999999999998224, 10.00000000000000000, -30.00000000000000355 ) ) ;
#12266 = FACE_OUTER_BOUND ( 'NONE', #1954, .T. ) ;
#12267 = ORIENTED_EDGE ( 'NONE', *, *, #13239, .F. ) ;
#12268 = DIRECTION ( 'NONE',  ( 0.000000000000000000, 0.000000000000000000, 1.000000000000000000 ) ) ;
#12269 = EDGE_LOOP ( 'NONE', ( #14801, #6358, #7146, #7588 ) ) ;
#12270 = DIRECTION ( 'NONE',  ( 0.000000000000000000, 0.000000000000000000, 1.000000000000000000 ) ) ;
#12271 = EDGE_LOOP ( 'NONE', ( #14315, #110 ) ) ;
#12272 = CARTESIAN_POINT ( 'NONE',  ( 27.48361012698968864, 136.6227766016838245, -4.651049393634109604E-13 ) ) ;
#12273 = VECTOR ( 'NONE', #8836, 1000.000000000000000 ) ;
#12274 = CARTESIAN_POINT ( 'NONE',  ( 27.75000000000000000, 0.000000000000000000, 0.000000000000000000 ) ) ;
#12275 = CIRCLE ( 'NONE', #13697, 2.499999999999998668 ) ;
#12276 = VERTEX_POINT ( 'NONE', #8336 ) ;
#12277 = DIRECTION ( 'NONE',  ( 0.000000000000000000, 0.000000000000000000, 1.000000000000000000 ) ) ;
#12278 = CARTESIAN_POINT ( 'NONE',  ( 36.00000000000002132, 146.6227766016838245, -16.00000000000000000 ) ) ;
#12279 = CARTESIAN_POINT ( 'NONE',  ( -100.0000000000000000, 171.6227766016838245, 0.000000000000000000 ) ) ;
#12280 = EDGE_CURVE ( 'NONE', #7907, #14936, #5438, .T. ) ;
#12281 = EDGE_CURVE ( 'NONE', #11114, #12895, #1626, .T. ) ;
#12282 = ADVANCED_FACE ( 'NONE', ( #12427, #296 ), #16500, .T. ) ;
#12283 = B_SPLINE_CURVE_WITH_KNOTS ( 'NONE', 3,
 ( #8537, #3223, #11100, #12699 ),
 .UNSPECIFIED., .F., .F.,
 ( 4, 4 ),
 ( 0.004999999999999983624, 0.009999999999999993269 ),
 .UNSPECIFIED. ) ;
#12284 = VECTOR ( 'NONE', #1788, 1000.000000000000000 ) ;
#12285 = CARTESIAN_POINT ( 'NONE',  ( 17.19546515351294147, 126.2270863594749670, -7.189547039408070717 ) ) ;
#12286 = CIRCLE ( 'NONE', #10014, 8.000000000000000000 ) ;
#12287 = ORIENTED_EDGE ( 'NONE', *, *, #15962, .T. ) ;
#12288 = FACE_BOUND ( 'NONE', #8187, .T. ) ;
#12289 = DIRECTION ( 'NONE',  ( -1.000000000000000000, -0.000000000000000000, 0.000000000000000000 ) ) ;
#12290 = ORIENTED_EDGE ( 'NONE', *, *, #16063, .T. ) ;
#12291 = CARTESIAN_POINT ( 'NONE',  ( -74.68241007762553352, 193.8375574372276162, -27.04711750382526603 ) ) ;
#12292 = DIRECTION ( 'NONE',  ( -1.000000000000000000, 0.000000000000000000, 0.000000000000000000 ) ) ;
#12293 = DIRECTION ( 'NONE',  ( -1.000000000000000000, -0.000000000000000000, -0.000000000000000000 ) ) ;
#12294 = DIRECTION ( 'NONE',  ( 0.000000000000000000, 1.000000000000000000, 0.000000000000000000 ) ) ;
#12295 = AXIS2_PLACEMENT_3D ( 'NONE', #4958, #1155, #7527 ) ;
#12296 = DIRECTION ( 'NONE',  ( 0.000000000000000000, 0.000000000000000000, -1.000000000000000000 ) ) ;
#12297 = CARTESIAN_POINT ( 'NONE',  ( -82.50000000000002842, 146.6227766016838245, 0.000000000000000000 ) ) ;
#12298 = LINE ( 'NONE', #11062, #15828 ) ;
#12299 = AXIS2_PLACEMENT_3D ( 'NONE', #13068, #7659, #11561 ) ;
#12300 =( LENGTH_UNIT ( ) NAMED_UNIT ( * ) SI_UNIT ( .MILLI., .METRE. ) );
#12301 = ORIENTED_EDGE ( 'NONE', *, *, #14691, .F. ) ;
#12302 = CARTESIAN_POINT ( 'NONE',  ( -8.091731396663927711, 30.16237610810089365, -15.00000000000000355 ) ) ;
#12303 = EDGE_CURVE ( 'NONE', #254, #12210, #3805, .T. ) ;
#12304 = EDGE_CURVE ( 'NONE', #13530, #16273, #5561, .T. ) ;
#12305 = ORIENTED_EDGE ( 'NONE', *, *, #9547, .T. ) ;
#12306 = DIRECTION ( 'NONE',  ( 0.000000000000000000, 0.000000000000000000, -1.000000000000000000 ) ) ;
#12307 = DIRECTION ( 'NONE',  ( 0.000000000000000000, 0.000000000000000000, -1.000000000000000000 ) ) ;
#12308 = VERTEX_POINT ( 'NONE', #17175 ) ;
#12309 = CARTESIAN_POINT ( 'NONE',  ( -15.09561842307794599, 19.99999999999308287, 7.342182892333040556 ) ) ;
#12310 = DIRECTION ( 'NONE',  ( 1.000000000000000000, -0.000000000000000000, 0.000000000000000000 ) ) ;
#12311 = AXIS2_PLACEMENT_3D ( 'NONE', #9963, #16794, #14222 ) ;
#12312 = ORIENTED_EDGE ( 'NONE', *, *, #2937, .F. ) ;
#12313 = AXIS2_PLACEMENT_3D ( 'NONE', #4591, #3080, #1755 ) ;
#12314 = CARTESIAN_POINT ( 'NONE',  ( 36.80614408739177179, 149.8074533144823874, -24.76648413410754657 ) ) ;
#12315 = AXIS2_PLACEMENT_3D ( 'NONE', #14254, #15320, #6107 ) ;
#12316 =( BOUNDED_SURFACE ( )  B_SPLINE_SURFACE ( 3, 2, ( 
 ( #15713, #9072, #14225 ),
 ( #5096, #4754, #10490 ),
 ( #14480, #2086, #14397 ),
 ( #6251, #3685, #15551 ) ),
 .UNSPECIFIED., .F., .F., .F. ) 
 B_SPLINE_SURFACE_WITH_KNOTS ( ( 4, 4 ),
 ( 3, 3 ),
 ( 0.1516087691302821228, 0.1566150273425061523 ),
 ( 0.000000000000000000, 1.000000000000000000 ),
 .UNSPECIFIED. ) 
 GEOMETRIC_REPRESENTATION_ITEM ( )  RATIONAL_B_SPLINE_SURFACE ( (
 ( 1.000000000000000000, 0.6556320892438535219, 1.000000000000000000),
 ( 1.000000000000000000, 0.6556321914870770762, 1.000000000000000000),
 ( 1.000000000000000000, 0.6556957163104851771, 1.000000000000000000),
 ( 1.000000000000000000, 0.6558243695371216431, 1.000000000000000000) ) ) 
 REPRESENTATION_ITEM ( '' )  SURFACE ( )  );
#12317 = VECTOR ( 'NONE', #5568, 1000.000000000000000 ) ;
#12318 = VERTEX_POINT ( 'NONE', #9200 ) ;
#12319 = LINE ( 'NONE', #10990, #1323 ) ;
#12320 = FACE_OUTER_BOUND ( 'NONE', #16906, .T. ) ;
#12321 = CYLINDRICAL_SURFACE ( 'NONE', #8524, 8.000000000000007105 ) ;
#12322 = ORIENTED_EDGE ( 'NONE', *, *, #6415, .F. ) ;
#12323 = FACE_OUTER_BOUND ( 'NONE', #8924, .T. ) ;
#12324 = EDGE_CURVE ( 'NONE', #2857, #1757, #2480, .T. ) ;
#12325 = AXIS2_PLACEMENT_3D ( 'NONE', #11614, #2139, #2227 ) ;
#12326 = AXIS2_PLACEMENT_3D ( 'NONE', #4472, #9857, #7803 ) ;
#12327 = VERTEX_POINT ( 'NONE', #16127 ) ;
#12328 = CARTESIAN_POINT ( 'NONE',  ( -80.00000000000001421, 196.6227766016838245, 0.000000000000000000 ) ) ;
#12329 = VECTOR ( 'NONE', #3230, 1000.000000000000000 ) ;
#12330 = ORIENTED_EDGE ( 'NONE', *, *, #3121, .T. ) ;
#12331 = CARTESIAN_POINT ( 'NONE',  ( -82.27956779150305522, 189.4719557769680591, -27.75644086540375000 ) ) ;
#12332 = DIRECTION ( 'NONE',  ( -1.000000000000000000, 0.000000000000000000, -8.673617379884037937E-17 ) ) ;
#12333 = CARTESIAN_POINT ( 'NONE',  ( -16.30611068361785954, 32.76923076923075939, -5.287877769756280877 ) ) ;
#12334 = AXIS2_PLACEMENT_3D ( 'NONE', #4071, #9630, #15112 ) ;
#12335 = ORIENTED_EDGE ( 'NONE', *, *, #10200, .F. ) ;
#12336 = ORIENTED_EDGE ( 'NONE', *, *, #1919, .F. ) ;
#12337 = CARTESIAN_POINT ( 'NONE',  ( 30.00000000000000355, 196.6227766016838245, 0.000000000000000000 ) ) ;
#12338 = CYLINDRICAL_SURFACE ( 'NONE', #12940, 2.500000000000000444 ) ;
#12339 = CARTESIAN_POINT ( 'NONE',  ( 12.97014296496520736, 138.3438685529228565, 12.30864880703445330 ) ) ;
#12340 = CIRCLE ( 'NONE', #13762, 33.00000000000000000 ) ;
#12341 = AXIS2_PLACEMENT_3D ( 'NONE', #10643, #16318, #17469 ) ;
#12342 = ORIENTED_EDGE ( 'NONE', *, *, #13761, .T. ) ;
#12343 = PRODUCT_CONTEXT ( 'NONE', #11840, 'mechanical' ) ;
#12344 = CARTESIAN_POINT ( 'NONE',  ( -45.00000000000000000, 130.0000000000000000, 15.00000000000000000 ) ) ;
#12345 = FACE_OUTER_BOUND ( 'NONE', #5287, .T. ) ;
#12346 = VECTOR ( 'NONE', #12553, 1000.000000000000000 ) ;
#12347 = CARTESIAN_POINT ( 'NONE',  ( 20.22365234301270931, 29.89465715177047400, -11.02453202869212312 ) ) ;
#12348 = CARTESIAN_POINT ( 'NONE',  ( -40.00000000000000000, 4.000000000000000000, -30.00000000000000711 ) ) ;
#12349 = DIRECTION ( 'NONE',  ( 0.000000000000000000, 0.000000000000000000, 1.000000000000000000 ) ) ;
#12350 = EDGE_CURVE ( 'NONE', #10830, #6313, #15453, .T. ) ;
#12351 = VERTEX_POINT ( 'NONE', #13457 ) ;
#12352 = CARTESIAN_POINT ( 'NONE',  ( -86.00000000000001421, 196.6227766016838245, -24.49489742783178770 ) ) ;
#12353 = CARTESIAN_POINT ( 'NONE',  ( -194.2319660531761656, 171.6227766016838245, 0.000000000000000000 ) ) ;
#12354 = FACE_OUTER_BOUND ( 'NONE', #15283, .T. ) ;
#12355 = DIRECTION ( 'NONE',  ( 0.000000000000000000, 0.000000000000000000, 1.000000000000000000 ) ) ;
#12356 = CARTESIAN_POINT ( 'NONE',  ( -40.00000000000000000, 0.000000000000000000, -40.00000000000000000 ) ) ;
#12357 = EDGE_LOOP ( 'NONE', ( #13174, #15785, #672, #3586 ) ) ;
#12358 = VECTOR ( 'NONE', #4337, 1000.000000000000000 ) ;
#12359 = EDGE_CURVE ( 'NONE', #17318, #3061, #15854, .T. ) ;
#12360 = EDGE_CURVE ( 'NONE', #6590, #11263, #13188, .T. ) ;
#12361 = PRESENTATION_LAYER_ASSIGNMENT (  '', '', ( #1347 ) ) ;
#12362 = LINE ( 'NONE', #8017, #14712 ) ;
#12363 = ORIENTED_EDGE ( 'NONE', *, *, #5442, .T. ) ;
#12364 = DIRECTION ( 'NONE',  ( 1.000000000000000000, -0.000000000000000000, -0.000000000000000000 ) ) ;
#12365 = ORIENTED_EDGE ( 'NONE', *, *, #5476, .T. ) ;
#12366 = CARTESIAN_POINT ( 'NONE',  ( -85.00000000000002842, 146.6227766016838245, 21.54065922853802562 ) ) ;
#12367 = CYLINDRICAL_SURFACE ( 'NONE', #9473, 5.000000000000007994 ) ;
#12368 = DIRECTION ( 'NONE',  ( 0.000000000000000000, 0.000000000000000000, -1.000000000000000000 ) ) ;
#12369 = AXIS2_PLACEMENT_3D ( 'NONE', #10917, #16435, #5528 ) ;
#12370 = AXIS2_PLACEMENT_3D ( 'NONE', #16123, #5043, #13366 ) ;
#12371 = ORIENTED_EDGE ( 'NONE', *, *, #9014, .F. ) ;
#12372 = CARTESIAN_POINT ( 'NONE',  ( 0.000000000000000000, 0.000000000000000000, 0.000000000000000000 ) ) ;
#12373 = FACE_OUTER_BOUND ( 'NONE', #11772, .T. ) ;
#12374 = FACE_BOUND ( 'NONE', #7885, .T. ) ;
#12375 = PRODUCT_DEFINITION_SHAPE ( 'NONE', 'NONE',  #4491 ) ;
#12376 = EDGE_CURVE ( 'NONE', #3419, #16407, #7809, .T. ) ;
#12377 = CARTESIAN_POINT ( 'NONE',  ( 17.54349574104657705, 125.4948194589026684, -5.000000000000002665 ) ) ;
#12378 = VECTOR ( 'NONE', #11452, 1000.000000000000000 ) ;
#12379 = ORIENTED_EDGE ( 'NONE', *, *, #741, .F. ) ;
#12380 = DIRECTION ( 'NONE',  ( -1.000000000000000000, -0.000000000000000000, -0.000000000000000000 ) ) ;
#12381 = AXIS2_PLACEMENT_3D ( 'NONE', #13985, #7081, #11132 ) ;
#12382 = PRESENTATION_LAYER_ASSIGNMENT (  '', '', ( #2787 ) ) ;
#12383 = CARTESIAN_POINT ( 'NONE',  ( -80.00000000000001421, 196.6227766016838245, 0.000000000000000000 ) ) ;
#12384 = VERTEX_POINT ( 'NONE', #10800 ) ;
#12385 =( LENGTH_UNIT ( ) NAMED_UNIT ( * ) SI_UNIT ( .MILLI., .METRE. ) );
#12386 = CARTESIAN_POINT ( 'NONE',  ( -32.43085388486101550, 119.6546501525790234, -5.312352691002971028 ) ) ;
#12387 = DIRECTION ( 'NONE',  ( 0.000000000000000000, 0.000000000000000000, -1.000000000000000000 ) ) ;
#12388 = EDGE_CURVE ( 'NONE', #15972, #4581, #5846, .T. ) ;
#12389 = CARTESIAN_POINT ( 'NONE',  ( 39.99999999999998579, 4.000000000000000000, 33.00000000000000711 ) ) ;
#12390 = CARTESIAN_POINT ( 'NONE',  ( 1.559999999999998943, 0.000000000000000000, 0.000000000000000000 ) ) ;
#12391 = DIRECTION ( 'NONE',  ( -1.000000000000000000, 0.000000000000000000, 0.000000000000000000 ) ) ;
#12392 = CARTESIAN_POINT ( 'NONE',  ( -725.0000000000000000, 130.0000000000000000, 13.00000000000000000 ) ) ;
#12393 = VECTOR ( 'NONE', #2838, 1000.000000000000000 ) ;
#12394 = FACE_OUTER_BOUND ( 'NONE', #2187, .T. ) ;
#12395 = CIRCLE ( 'NONE', #13258, 5.315148208181398104 ) ;
#12396 = ORIENTED_EDGE ( 'NONE', *, *, #9808, .F. ) ;
#12397 = LINE ( 'NONE', #16397, #13536 ) ;
#12398 = ORIENTED_EDGE ( 'NONE', *, *, #10741, .F. ) ;
#12399 = CARTESIAN_POINT ( 'NONE',  ( 34.42312820345349422, 19.99999999999999645, -9.539278825327816236 ) ) ;
#12400 = CARTESIAN_POINT ( 'NONE',  ( 15.78015847649388448, 143.0439382767918346, -16.49999999999050360 ) ) ;
#12401 = VERTEX_POINT ( 'NONE', #11948 ) ;
#12402 = AXIS2_PLACEMENT_3D ( 'NONE', #9687, #9867, #15085 ) ;
#12403 = CARTESIAN_POINT ( 'NONE',  ( -23.00000000000002132, 100.0000000000000142, 4.999999999999999112 ) ) ;
#12404 = DIRECTION ( 'NONE',  ( -0.000000000000000000, -0.000000000000000000, -1.000000000000000000 ) ) ;
#12405 = VECTOR ( 'NONE', #12917, 1000.000000000000000 ) ;
#12406 = ORIENTED_EDGE ( 'NONE', *, *, #17427, .F. ) ;
#12407 = VECTOR ( 'NONE', #8700, 1000.000000000000000 ) ;
#12408 = CARTESIAN_POINT ( 'NONE',  ( 25.53529511534545549, 152.6548696709631372, -27.00480063125522889 ) ) ;
#12409 = AXIS2_PLACEMENT_3D ( 'NONE', #10048, #10143, #14145 ) ;
#12410 = DIRECTION ( 'NONE',  ( -0.000000000000000000, -0.000000000000000000, 1.000000000000000000 ) ) ;
#12411 = EDGE_CURVE ( 'NONE', #11461, #8974, #17444, .T. ) ;
#12412 = EDGE_CURVE ( 'NONE', #8580, #5427, #17349, .T. ) ;
#12413 = EDGE_CURVE ( 'NONE', #3299, #10402, #5220, .T. ) ;
#12414 = CARTESIAN_POINT ( 'NONE',  ( -153.0000000000000284, 171.6227766016838245, -11.93698985866628526 ) ) ;
#12415 = CARTESIAN_POINT ( 'NONE',  ( -103.0000000000000142, 171.6227766016838245, 0.000000000000000000 ) ) ;
#12416 = CARTESIAN_POINT ( 'NONE',  ( 35.00000000000000000, 196.6227766016838245, -35.00200000000000244 ) ) ;
#12417 = DIRECTION ( 'NONE',  ( 0.000000000000000000, 0.000000000000000000, -1.000000000000000000 ) ) ;
#12418 = DIRECTION ( 'NONE',  ( 0.000000000000000000, 0.000000000000000000, -1.000000000000000000 ) ) ;
#12419 = ORIENTED_EDGE ( 'NONE', *, *, #16165, .T. ) ;
#12420 = CARTESIAN_POINT ( 'NONE',  ( 12.22466323754103001, 142.0699085367067767, -18.75233045409083843 ) ) ;
#12421 = AXIS2_PLACEMENT_3D ( 'NONE', #3016, #8507, #13918 ) ;
#12422 = CIRCLE ( 'NONE', #5650, 33.00000000000000000 ) ;
#12423 = AXIS2_PLACEMENT_3D ( 'NONE', #7706, #7538, #10456 ) ;
#12424 = ORIENTED_EDGE ( 'NONE', *, *, #1533, .F. ) ;
#12425 = DIRECTION ( 'NONE',  ( 0.000000000000000000, 0.000000000000000000, 1.000000000000000000 ) ) ;
#12426 = CIRCLE ( 'NONE', #13285, 2.500000000000002220 ) ;
#12427 = FACE_OUTER_BOUND ( 'NONE', #7799, .T. ) ;
#12428 = DIRECTION ( 'NONE',  ( -1.000000000000000000, -0.000000000000000000, -0.000000000000000000 ) ) ;
#12429 = ORIENTED_EDGE ( 'NONE', *, *, #5159, .F. ) ;
#12430 = ORIENTED_EDGE ( 'NONE', *, *, #2930, .T. ) ;
#12431 = CYLINDRICAL_SURFACE ( 'NONE', #6064, 20.00000000000000355 ) ;
#12432 = DIRECTION ( 'NONE',  ( 1.000000000000000000, 0.000000000000000000, 0.000000000000000000 ) ) ;
#12433 = CARTESIAN_POINT ( 'NONE',  ( 19.90854668962809626, 140.2883655178033848, 15.59737012465792461 ) ) ;
#12434 = CIRCLE ( 'NONE', #17244, 4.750000000000000000 ) ;
#12435 = ORIENTED_EDGE ( 'NONE', *, *, #11712, .T. ) ;
#12436 = DIRECTION ( 'NONE',  ( 0.000000000000000000, 0.000000000000000000, 1.000000000000000000 ) ) ;
#12437 = CIRCLE ( 'NONE', #9610, 33.00000000000000000 ) ;
#12438 = CARTESIAN_POINT ( 'NONE',  ( -100.0000000000000000, 143.0439382767972347, -16.49999999999984368 ) ) ;
#12439 = CARTESIAN_POINT ( 'NONE',  ( 16.75836516268004317, 29.96322345091821049, -12.79344305462037035 ) ) ;
#12440 = CARTESIAN_POINT ( 'NONE',  ( 15.60228996708978855, 124.9392590763941371, 1.671781470417840199 ) ) ;
#12441 = CYLINDRICAL_SURFACE ( 'NONE', #15168, 1.000000000000000888 ) ;
#12442 = EDGE_LOOP ( 'NONE', ( #17117, #1472, #17325, #12577 ) ) ;
#12443 = DIRECTION ( 'NONE',  ( -1.000000000000000000, -0.000000000000000000, -0.000000000000000000 ) ) ;
#12444 = CARTESIAN_POINT ( 'NONE',  ( -32.99999999999998579, 10.00000000000000000, 0.000000000000000000 ) ) ;
#12445 = CARTESIAN_POINT ( 'NONE',  ( 30.00000000000001066, 146.6227766016838245, -16.00000000000000000 ) ) ;
#12446 = DIRECTION ( 'NONE',  ( 8.673617379884037937E-17, 0.000000000000000000, 1.000000000000000000 ) ) ;
#12447 = DIRECTION ( 'NONE',  ( 0.8571673013836867971, 1.049727191973306626E-16, -0.5150380737757237481 ) ) ;
#12448 = PRODUCT_DEFINITION_CONTEXT ( 'detailed design', #12523, 'design' ) ;
#12449 = CIRCLE ( 'NONE', #11305, 10.00000000000000000 ) ;
#12450 = VECTOR ( 'NONE', #4238, 1000.000000000000000 ) ;
#12451 = ORIENTED_EDGE ( 'NONE', *, *, #6385, .T. ) ;
#12452 = ORIENTED_EDGE ( 'NONE', *, *, #9532, .T. ) ;
#12453 = VECTOR ( 'NONE', #6803, 1000.000000000000000 ) ;
#12454 = CARTESIAN_POINT ( 'NONE',  ( 13.53786153804126435, 143.5554826938402755, 17.35616514752890183 ) ) ;
#12455 = VERTEX_POINT ( 'NONE', #4076 ) ;
#12456 = EDGE_CURVE ( 'NONE', #15728, #9063, #2445, .T. ) ;
#12457 = CARTESIAN_POINT ( 'NONE',  ( 48.00000000000000711, 167.6227766016838814, -16.92820660268601429 ) ) ;
#12458 = ORIENTED_EDGE ( 'NONE', *, *, #2454, .T. ) ;
#12459 = DIRECTION ( 'NONE',  ( 0.000000000000000000, 1.000000000000000000, 0.000000000000000000 ) ) ;
#12460 = CARTESIAN_POINT ( 'NONE',  ( -95.00000000000000000, 199.3133755249253056, -1.695560166891042033E-15 ) ) ;
#12461 = CARTESIAN_POINT ( 'NONE',  ( -45.00000000000000000, 130.0000000000000000, -15.00000000000000000 ) ) ;
#12462 = VECTOR ( 'NONE', #13420, 1000.000000000000000 ) ;
#12463 = CARTESIAN_POINT ( 'NONE',  ( 35.89206792073697017, 141.9594008680238062, -14.48313018527312046 ) ) ;
#12464 = CIRCLE ( 'NONE', #7633, 7.500000000000000000 ) ;
#12465 = VERTEX_POINT ( 'NONE', #5047 ) ;
#12466 = CYLINDRICAL_SURFACE ( 'NONE', #5872, 5.000000000000007994 ) ;
#12467 = DIRECTION ( 'NONE',  ( 1.000000000000000000, 0.000000000000000000, 0.000000000000000000 ) ) ;
#12468 = CARTESIAN_POINT ( 'NONE',  ( -85.00000000000002842, 196.6227766016838245, 21.54065922853802562 ) ) ;
#12469 = CARTESIAN_POINT ( 'NONE',  ( 49.99999999999998579, 167.6227766016838814, -19.42820660268601074 ) ) ;
#12470 = CARTESIAN_POINT ( 'NONE',  ( 15.82262738632537946, 137.2266821760960340, -8.447647312139547893 ) ) ;
#12471 = ORIENTED_EDGE ( 'NONE', *, *, #8828, .F. ) ;
#12472 = EDGE_CURVE ( 'NONE', #16355, #11917, #7261, .T. ) ;
#12473 = CARTESIAN_POINT ( 'NONE',  ( -75.17527926758620538, 150.2116474542519882, -27.68948087834226612 ) ) ;
#12474 = DIRECTION ( 'NONE',  ( -0.000000000000000000, -0.000000000000000000, 1.000000000000000000 ) ) ;
#12475 = ORIENTED_EDGE ( 'NONE', *, *, #6923, .F. ) ;
#12476 = CARTESIAN_POINT ( 'NONE',  ( -84.82038104795840638, 193.0449522123385862, -27.67906398090707754 ) ) ;
#12477 = CARTESIAN_POINT ( 'NONE',  ( -91.33974596215561803, 206.6227766016838245, 0.000000000000000000 ) ) ;
#12478 = EDGE_CURVE ( 'NONE', #12567, #10750, #10359, .T. ) ;
#12479 = DIRECTION ( 'NONE',  ( -1.000000000000000000, -6.938893903907228378E-16, -0.000000000000000000 ) ) ;
#12480 = EDGE_CURVE ( 'NONE', #544, #1967, #15864, .T. ) ;
#12481 = DIRECTION ( 'NONE',  ( 0.000000000000000000, 0.000000000000000000, 1.000000000000000000 ) ) ;
#12482 = EDGE_CURVE ( 'NONE', #10010, #14157, #15118, .T. ) ;
#12483 = CARTESIAN_POINT ( 'NONE',  ( -3.000000000000000888, 154.3022685259950038, 9.999999999999900524 ) ) ;
#12484 = AXIS2_PLACEMENT_3D ( 'NONE', #13771, #7389, #3222 ) ;
#12485 = CARTESIAN_POINT ( 'NONE',  ( 48.00000000000000711, 167.6227766016838814, 21.92820660268601074 ) ) ;
#12486 = CARTESIAN_POINT ( 'NONE',  ( -80.25919237425941333, 201.6174249061529054, 13.75941557453014497 ) ) ;
#12487 =( NAMED_UNIT ( * ) PLANE_ANGLE_UNIT ( ) SI_UNIT ( $, .RADIAN. ) );
#12488 = ORIENTED_EDGE ( 'NONE', *, *, #16551, .F. ) ;
#12489 = ORIENTED_EDGE ( 'NONE', *, *, #17517, .T. ) ;
#12490 = FACE_OUTER_BOUND ( 'NONE', #421, .T. ) ;
#12491 = FACE_OUTER_BOUND ( 'NONE', #16790, .T. ) ;
#12492 = ADVANCED_FACE ( 'NONE', ( #9903 ), #1589, .T. ) ;
#12493 = ORIENTED_EDGE ( 'NONE', *, *, #7119, .T. ) ;
#12494 = DIRECTION ( 'NONE',  ( 0.000000000000000000, 0.000000000000000000, -1.000000000000000000 ) ) ;
#12495 = CARTESIAN_POINT ( 'NONE',  ( -153.0000000000000284, 171.6227766016838245, 0.000000000000000000 ) ) ;
#12496 = ORIENTED_EDGE ( 'NONE', *, *, #5294, .F. ) ;
#12497 = CARTESIAN_POINT ( 'NONE',  ( 23.91032892519173458, 151.0287754819114241, -25.78994361341036168 ) ) ;
#12498 = DIRECTION ( 'NONE',  ( -1.000000000000000000, 0.000000000000000000, 0.000000000000000000 ) ) ;
#12499 = FACE_OUTER_BOUND ( 'NONE', #12269, .T. ) ;
#12500 = CARTESIAN_POINT ( 'NONE',  ( 27.99999999999998224, 9.999999999999998224, 1.387778780781445676E-14 ) ) ;
#12501 = CARTESIAN_POINT ( 'NONE',  ( -77.50000000000002842, 146.6227766016838245, 0.000000000000000000 ) ) ;
#12502 = CARTESIAN_POINT ( 'NONE',  ( -23.00000000000000000, 120.0000000000000284, 0.000000000000000000 ) ) ;
#12503 = DIRECTION ( 'NONE',  ( -0.000000000000000000, -1.000000000000000000, 0.000000000000000000 ) ) ;
#12504 = VERTEX_POINT ( 'NONE', #12389 ) ;
#12505 = CARTESIAN_POINT ( 'NONE',  ( 27.44407568426044364, 136.8394969516870958, -3.888888888888887063 ) ) ;
#12506 = ORIENTED_EDGE ( 'NONE', *, *, #12350, .F. ) ;
#12507 = DIRECTION ( 'NONE',  ( -0.000000000000000000, -1.000000000000000000, -0.000000000000000000 ) ) ;
#12508 = ADVANCED_FACE ( 'NONE', ( #16388 ), #5747, .T. ) ;
#12509 = ORIENTED_EDGE ( 'NONE', *, *, #13936, .F. ) ;
#12510 = EDGE_CURVE ( 'NONE', #15648, #8600, #16022, .T. ) ;
#12511 = ORIENTED_EDGE ( 'NONE', *, *, #12091, .F. ) ;
#12512 = EDGE_CURVE ( 'NONE', #4990, #5007, #15035, .T. ) ;
#12513 = VERTEX_POINT ( 'NONE', #11230 ) ;
#12514 = CARTESIAN_POINT ( 'NONE',  ( -3.000000000000000888, 171.6227766016838245, 0.000000000000000000 ) ) ;
#12515 = EDGE_CURVE ( 'NONE', #8018, #15354, #4254, .T. ) ;
#12516 = FACE_OUTER_BOUND ( 'NONE', #2840, .T. ) ;
#12517 = CARTESIAN_POINT ( 'NONE',  ( 14.17453072134883030, 137.9246278893784847, 11.09209212451273707 ) ) ;
#12518 = ORIENTED_EDGE ( 'NONE', *, *, #11598, .F. ) ;
#12519 = LINE ( 'NONE', #9856, #13244 ) ;
#12520 = CARTESIAN_POINT ( 'NONE',  ( -27.98221281347036893, 30.00000000000000355, 4.999999999999999112 ) ) ;
#12521 = CARTESIAN_POINT ( 'NONE',  ( -81.53182587509584778, 191.8593874686152105, 26.06696055488265529 ) ) ;
#12522 = CARTESIAN_POINT ( 'NONE',  ( 225.0000000000000000, 89.99999999999997158, 4.999999999999999112 ) ) ;
#12523 = APPLICATION_CONTEXT ( 'automotive_design' ) ;
#12524 = CARTESIAN_POINT ( 'NONE',  ( 14.93242934743710570, 18.00000000000000355, 12.99999999999999822 ) ) ;
#12525 = DIRECTION ( 'NONE',  ( 0.000000000000000000, 0.000000000000000000, -1.000000000000000000 ) ) ;
#12526 = EDGE_LOOP ( 'NONE', ( #3106, #958, #13123, #1643 ) ) ;
#12527 = CARTESIAN_POINT ( 'NONE',  ( 27.47046400057530846, 138.6909045376442009, -2.448381753924629756 ) ) ;
#12528 = DIRECTION ( 'NONE',  ( -0.000000000000000000, -0.000000000000000000, 1.000000000000000000 ) ) ;
#12529 = CARTESIAN_POINT ( 'NONE',  ( 25.51458778375578973, 19.99999999999999289, -21.98440010584615578 ) ) ;
#12530 = FACE_OUTER_BOUND ( 'NONE', #7185, .T. ) ;
#12531 = LINE ( 'NONE', #1738, #8076 ) ;
#12532 = EDGE_LOOP ( 'NONE', ( #5235, #6067, #3417, #7821, #6219, #11962 ) ) ;
#12533 = EDGE_CURVE ( 'NONE', #3871, #4327, #2163, .T. ) ;
#12534 = ORIENTED_EDGE ( 'NONE', *, *, #3992, .T. ) ;
#12535 = EDGE_CURVE ( 'NONE', #14250, #9898, #13767, .T. ) ;
#12536 = CARTESIAN_POINT ( 'NONE',  ( 8.147273376221958685, 133.4207317082267537, 12.78321197947435728 ) ) ;
#12537 = ORIENTED_EDGE ( 'NONE', *, *, #14791, .T. ) ;
#12538 = CARTESIAN_POINT ( 'NONE',  ( -27.99999999999998224, 10.00000000000000000, -16.00000000000000000 ) ) ;
#12539 = ORIENTED_EDGE ( 'NONE', *, *, #15307, .F. ) ;
#12540 = DIRECTION ( 'NONE',  ( -1.000000000000000000, -0.000000000000000000, 0.000000000000000000 ) ) ;
#12541 = DIRECTION ( 'NONE',  ( 0.000000000000000000, 0.000000000000000000, 1.000000000000000000 ) ) ;
#12542 = DIRECTION ( 'NONE',  ( 0.000000000000000000, 1.000000000000000000, 1.224646799147353207E-16 ) ) ;
#12543 = CARTESIAN_POINT ( 'NONE',  ( -16.30611068361787019, 32.76923076923078781, 0.000000000000000000 ) ) ;
#12544 = CARTESIAN_POINT ( 'NONE',  ( 29.97257796258590901, 18.00000000000000000, -18.20111186907413980 ) ) ;
#12545 = ORIENTED_EDGE ( 'NONE', *, *, #16680, .T. ) ;
#12546 = DIRECTION ( 'NONE',  ( 0.000000000000000000, 0.000000000000000000, -1.000000000000000000 ) ) ;
#12547 = CARTESIAN_POINT ( 'NONE',  ( -20.00000000000000355, 171.6227766016838245, 0.000000000000000000 ) ) ;
#12548 = LINE ( 'NONE', #7325, #15565 ) ;
#12549 = EDGE_CURVE ( 'NONE', #1245, #10869, #9815, .T. ) ;
#12550 = DIRECTION ( 'NONE',  ( -1.000000000000000000, 0.000000000000000000, 0.000000000000000000 ) ) ;
#12551 = FACE_BOUND ( 'NONE', #8278, .T. ) ;
#12552 = ORIENTED_EDGE ( 'NONE', *, *, #3862, .F. ) ;
#12553 = DIRECTION ( 'NONE',  ( 0.000000000000000000, -1.000000000000000000, 0.000000000000000000 ) ) ;
#12554 = CIRCLE ( 'NONE', #6621, 2.499999999999999556 ) ;
#12555 = EDGE_LOOP ( 'NONE', ( #13624, #1149 ) ) ;
#12556 = PRESENTATION_STYLE_ASSIGNMENT (( #7158 ) ) ;
#12557 = FACE_OUTER_BOUND ( 'NONE', #16825, .T. ) ;
#12558 = FACE_OUTER_BOUND ( 'NONE', #8973, .T. ) ;
#12559 = CARTESIAN_POINT ( 'NONE',  ( 196.0000000000000000, 163.6227766016838530, -15.00000337241049486 ) ) ;
#12560 = DIRECTION ( 'NONE',  ( 0.000000000000000000, 0.000000000000000000, -1.000000000000000000 ) ) ;
#12561 = CYLINDRICAL_SURFACE ( 'NONE', #11786, 30.00000000000000000 ) ;
#12562 = CARTESIAN_POINT ( 'NONE',  ( -100.0000000000000000, 171.6227766016838245, 0.000000000000000000 ) ) ;
#12563 = CARTESIAN_POINT ( 'NONE',  ( -81.74336020400447467, 201.3127097690254175, 14.40604465277978541 ) ) ;
#12564 = EDGE_CURVE ( 'NONE', #2136, #4295, #424, .T. ) ;
#12565 = FACE_BOUND ( 'NONE', #14304, .T. ) ;
#12566 = AXIS2_PLACEMENT_3D ( 'NONE', #1069, #6470, #9207 ) ;
#12567 = VERTEX_POINT ( 'NONE', #16649 ) ;
#12568 = AXIS2_PLACEMENT_3D ( 'NONE', #12770, #12503, #3204 ) ;
#12569 = EDGE_LOOP ( 'NONE', ( #14237, #1353, #7789, #14069, #10518 ) ) ;
#12570 = CARTESIAN_POINT ( 'NONE',  ( 34.26467700469002864, 19.99999999999999645, -10.17319632352553427 ) ) ;
#12571 = DIRECTION ( 'NONE',  ( -0.000000000000000000, -0.000000000000000000, -1.000000000000000000 ) ) ;
#12572 = ORIENTED_EDGE ( 'NONE', *, *, #15983, .T. ) ;
#12573 = EDGE_CURVE ( 'NONE', #14342, #9691, #17439, .T. ) ;
#12574 = DIRECTION ( 'NONE',  ( 0.000000000000000000, 0.000000000000000000, -1.000000000000000000 ) ) ;
#12575 = EDGE_CURVE ( 'NONE', #11867, #5256, #15806, .T. ) ;
#12576 = CARTESIAN_POINT ( 'NONE',  ( 196.0000000000000000, 163.6227766016838530, 12.50000337241049309 ) ) ;
#12577 = ORIENTED_EDGE ( 'NONE', *, *, #10165, .F. ) ;
#12578 = CARTESIAN_POINT ( 'NONE',  ( 34.26947555605809015, 152.8115259536290864, -27.11642929875283059 ) ) ;
#12579 = AXIS2_PLACEMENT_3D ( 'NONE', #4876, #15856, #17177 ) ;
#12580 = CARTESIAN_POINT ( 'NONE',  ( -12.63167751028164965, 18.00000000000000000, 24.35243221814330994 ) ) ;
#12581 = VECTOR ( 'NONE', #8482, 1000.000000000000000 ) ;
#12582 = CARTESIAN_POINT ( 'NONE',  ( -70.00000000000000000, 191.6227766016837961, 1.224646799147353454E-15 ) ) ;
#12583 = DIRECTION ( 'NONE',  ( 0.9961946980917461003, -0.04357787137382522491, -0.07547908730516825204 ) ) ;
#12584 = FACE_OUTER_BOUND ( 'NONE', #2853, .T. ) ;
#12585 = CARTESIAN_POINT ( 'NONE',  ( 17.54349574104648823, 125.4948194589026684, -4.999999999999997335 ) ) ;
#12586 = CARTESIAN_POINT ( 'NONE',  ( 17.00000000000000000, 171.6227766016838245, 0.000000000000000000 ) ) ;
#12587 = EDGE_LOOP ( 'NONE', ( #12832, #12305, #10312, #13479 ) ) ;
#12588 = CARTESIAN_POINT ( 'NONE',  ( 10.42241938378121624, 142.2974014187406055, -19.10582184898306224 ) ) ;
#12589 = ORIENTED_EDGE ( 'NONE', *, *, #10443, .F. ) ;
#12590 = FACE_OUTER_BOUND ( 'NONE', #3491, .T. ) ;
#12591 = ADVANCED_FACE ( 'NONE', ( #4913 ), #3684, .T. ) ;
#12592 = DIRECTION ( 'NONE',  ( 0.000000000000000000, -1.000000000000000000, 6.123233995736762338E-17 ) ) ;
#12593 =( GEOMETRIC_REPRESENTATION_CONTEXT ( 3 ) GLOBAL_UNCERTAINTY_ASSIGNED_CONTEXT ( ( #6505 ) ) GLOBAL_UNIT_ASSIGNED_CONTEXT ( ( #6976, #16725, #11044 ) ) REPRESENTATION_CONTEXT ( 'NONE', 'WORKASPACE' ) );
#12594 = ORIENTED_EDGE ( 'NONE', *, *, #6936, .T. ) ;
#12595 = VERTEX_POINT ( 'NONE', #15712 ) ;
#12596 = CARTESIAN_POINT ( 'NONE',  ( -3.000000000000002665, 171.6227766016838245, 0.000000000000000000 ) ) ;
#12597 = AXIS2_PLACEMENT_3D ( 'NONE', #181, #9212, #2923 ) ;
#12598 = CARTESIAN_POINT ( 'NONE',  ( -68.00000000000000000, 171.6227766016838245, 0.000000000000000000 ) ) ;
#12599 = CARTESIAN_POINT ( 'NONE',  ( 14.91849273675205545, 128.9263856399286396, 11.14803070335530855 ) ) ;
#12600 = EDGE_LOOP ( 'NONE', ( #13117, #13200 ) ) ;
#12601 = CARTESIAN_POINT ( 'NONE',  ( -70.00000000000000000, 171.6227766016838245, 0.000000000000000000 ) ) ;
#12602 = CARTESIAN_POINT ( 'NONE',  ( -208.3486229709906752, 168.0754701982166068, -6.144114920819716552 ) ) ;
#12603 = AXIS2_PLACEMENT_3D ( 'NONE', #13587, #9668, #16425 ) ;
#12604 = AXIS2_PLACEMENT_3D ( 'NONE', #10370, #10547, #2409 ) ;
#12605 = FACE_OUTER_BOUND ( 'NONE', #665, .T. ) ;
#12606 = CARTESIAN_POINT ( 'NONE',  ( 27.99999999999998224, 9.999999999999998224, 1.387778780781445676E-14 ) ) ;
#12607 = EDGE_CURVE ( 'NONE', #12225, #10138, #5933, .T. ) ;
#12608 = CARTESIAN_POINT ( 'NONE',  ( 16.62686111071178630, 17.99999999999885603, 12.85442640772723344 ) ) ;
#12609 = AXIS2_PLACEMENT_3D ( 'NONE', #10237, #868, #12901 ) ;
#12610 = ORIENTED_EDGE ( 'NONE', *, *, #305, .F. ) ;
#12611 = DIRECTION ( 'NONE',  ( -0.000000000000000000, 0.8660254037844432595, -0.4999999999999919509 ) ) ;
#12612 = DIRECTION ( 'NONE',  ( 1.000000000000000000, 0.000000000000000000, -8.673617379884037937E-17 ) ) ;
#12613 = CYLINDRICAL_SURFACE ( 'NONE', #11993, 2.499999999999998668 ) ;
#12614 = LINE ( 'NONE', #666, #9861 ) ;
#12615 = LINE ( 'NONE', #2885, #4416 ) ;
#12616 = VERTEX_POINT ( 'NONE', #2344 ) ;
#12617 = VERTEX_POINT ( 'NONE', #11325 ) ;
#12618 = AXIS2_PLACEMENT_3D ( 'NONE', #10273, #8701, #4807 ) ;
#12619 = VECTOR ( 'NONE', #8593, 1000.000000000000000 ) ;
#12620 = CARTESIAN_POINT ( 'NONE',  ( 8.904477399773945479, 144.1137579919043787, 18.22932967255391290 ) ) ;
#12621 = VECTOR ( 'NONE', #15067, 1000.000000000000000 ) ;
#12622 = EDGE_LOOP ( 'NONE', ( #4089, #6979, #8404, #2322 ) ) ;
#12623 = ORIENTED_EDGE ( 'NONE', *, *, #3975, .F. ) ;
#12624 = SURFACE_SIDE_STYLE ('',( #595 ) ) ;
#12625 = DIRECTION ( 'NONE',  ( -1.000000000000000000, 0.000000000000000000, 0.000000000000000000 ) ) ;
#12626 = FACE_OUTER_BOUND ( 'NONE', #13691, .T. ) ;
#12627 = EDGE_CURVE ( 'NONE', #5354, #583, #9071, .T. ) ;
#12628 = ADVANCED_FACE ( 'NONE', ( #10489 ), #9939, .T. ) ;
#12629 = DIRECTION ( 'NONE',  ( 0.000000000000000000, 1.000000000000000000, 2.312964634635742267E-15 ) ) ;
#12630 = EDGE_CURVE ( 'NONE', #978, #8489, #12283, .T. ) ;
#12631 = ADVANCED_FACE ( 'NONE', ( #8450 ), #12441, .T. ) ;
#12632 = CIRCLE ( 'NONE', #16304, 11.99999999999999645 ) ;
#12633 = CIRCLE ( 'NONE', #15462, 2.500000000000002220 ) ;
#12634 = ORIENTED_EDGE ( 'NONE', *, *, #9045, .T. ) ;
#12635 = CARTESIAN_POINT ( 'NONE',  ( 32.50000000000000000, 196.6227766016838245, 10.00000000000000178 ) ) ;
#12636 = CARTESIAN_POINT ( 'NONE',  ( 39.99999999999998579, 0.000000000000000000, -30.00000000000001066 ) ) ;
#12637 = AXIS2_PLACEMENT_3D ( 'NONE', #6988, #12479, #3001 ) ;
#12638 = CYLINDRICAL_SURFACE ( 'NONE', #9897, 30.00000000000000000 ) ;
#12639 =( GEOMETRIC_REPRESENTATION_CONTEXT ( 3 ) GLOBAL_UNCERTAINTY_ASSIGNED_CONTEXT ( ( #4704 ) ) GLOBAL_UNIT_ASSIGNED_CONTEXT ( ( #1825, #14055, #11384 ) ) REPRESENTATION_CONTEXT ( 'NONE', 'WORKASPACE' ) );
#12640 = CARTESIAN_POINT ( 'NONE',  ( 196.0000000000000000, 163.6227766016838530, -12.50000337241049309 ) ) ;
#12641 = AXIS2_PLACEMENT_3D ( 'NONE', #13902, #12380, #9449 ) ;
#12642 = DIRECTION ( 'NONE',  ( 0.000000000000000000, 0.000000000000000000, 1.000000000000000000 ) ) ;
#12643 = EDGE_LOOP ( 'NONE', ( #15185, #3353 ) ) ;
#12644 = CARTESIAN_POINT ( 'NONE',  ( 27.48361012698969930, 136.6227766016838245, -1.296296296296295614 ) ) ;
#12645 = EDGE_LOOP ( 'NONE', ( #5661, #4574 ) ) ;
#12646 =( NAMED_UNIT ( * ) PLANE_ANGLE_UNIT ( ) SI_UNIT ( $, .RADIAN. ) );
#12647 = AXIS2_PLACEMENT_3D ( 'NONE', #9460, #1591, #11059 ) ;
#12648 = DIRECTION ( 'NONE',  ( 0.000000000000000000, 0.000000000000000000, 1.000000000000000000 ) ) ;
#12649 = ORIENTED_EDGE ( 'NONE', *, *, #12954, .F. ) ;
#12650 = CYLINDRICAL_SURFACE ( 'NONE', #16923, 10.00000000000000000 ) ;
#12651 =( REPRESENTATION_RELATIONSHIP ('NONE','NONE', #9723, #6585 ) REPRESENTATION_RELATIONSHIP_WITH_TRANSFORMATION ( #652 )SHAPE_REPRESENTATION_RELATIONSHIP( ) );
#12652 = CARTESIAN_POINT ( 'NONE',  ( 27.13959012325753406, 18.00000000000000000, 20.89788123228700556 ) ) ;
#12653 = CARTESIAN_POINT ( 'NONE',  ( -22.99999999999998224, 10.00000000000000000, 28.00000000000000355 ) ) ;
#12654 = ORIENTED_EDGE ( 'NONE', *, *, #12359, .T. ) ;
#12655 = CARTESIAN_POINT ( 'NONE',  ( -80.00000000000002842, 146.6227766016838245, 0.000000000000000000 ) ) ;
#12656 = CARTESIAN_POINT ( 'NONE',  ( 22.66773460012013430, 29.84724857135450193, 7.067878044979525320 ) ) ;
#12657 = CARTESIAN_POINT ( 'NONE',  ( -76.36262084616922152, 200.0658281092903508, 16.73852573662796317 ) ) ;
#12658 = ORIENTED_EDGE ( 'NONE', *, *, #16449, .T. ) ;
#12659 = ORIENTED_EDGE ( 'NONE', *, *, #11422, .F. ) ;
#12660 = CARTESIAN_POINT ( 'NONE',  ( 24.02621431236828187, 19.99999999999999645, -9.488192989094725860 ) ) ;
#12661 = AXIS2_PLACEMENT_3D ( 'NONE', #7918, #10386, #11895 ) ;
#12662 = LINE ( 'NONE', #11503, #6407 ) ;
#12663 = EDGE_LOOP ( 'NONE', ( #14472, #11052, #13504, #17338 ) ) ;
#12664 = DIRECTION ( 'NONE',  ( 1.000000000000000000, 0.000000000000000000, 0.000000000000000000 ) ) ;
#12665 = CARTESIAN_POINT ( 'NONE',  ( 49.99999999999998579, 167.6227766016838814, 19.42820660268601074 ) ) ;
#12666 = EDGE_LOOP ( 'NONE', ( #10157, #1186, #10289, #6137 ) ) ;
#12667 = EDGE_CURVE ( 'NONE', #9322, #9733, #6703, .T. ) ;
#12668 = PRODUCT_DEFINITION_SHAPE ( 'NONE', 'NONE',  #17533 ) ;
#12669 = FACE_OUTER_BOUND ( 'NONE', #3035, .T. ) ;
#12670 = ADVANCED_FACE ( 'NONE', ( #1641 ), #13772, .F. ) ;
#12671 = DIRECTION ( 'NONE',  ( -1.000000000000000000, 0.000000000000000000, 0.000000000000000000 ) ) ;
#12672 = AXIS2_PLACEMENT_3D ( 'NONE', #13130, #15689, #7463 ) ;
#12673 = CIRCLE ( 'NONE', #5036, 1.500000000000000000 ) ;
#12674 = CARTESIAN_POINT ( 'NONE',  ( -208.0706889292729045, 166.1570757162849077, -1.826518625235456383 ) ) ;
#12675 =( GEOMETRIC_REPRESENTATION_CONTEXT ( 3 ) GLOBAL_UNCERTAINTY_ASSIGNED_CONTEXT ( ( #11418 ) ) GLOBAL_UNIT_ASSIGNED_CONTEXT ( ( #6618, #10505, #10321 ) ) REPRESENTATION_CONTEXT ( 'NONE', 'WORKASPACE' ) );
#12676 = FACE_OUTER_BOUND ( 'NONE', #15576, .T. ) ;
#12677 = LINE ( 'NONE', #15057, #16737 ) ;
#12678 = CARTESIAN_POINT ( 'NONE',  ( -48.00000000000000000, 191.6227766016837961, -1.224646799147353454E-15 ) ) ;
#12679 = ADVANCED_FACE ( 'NONE', ( #312 ), #3318, .F. ) ;
#12680 = CARTESIAN_POINT ( 'NONE',  ( -72.56345771982930160, 145.5167101299680610, -20.20458554073935886 ) ) ;
#12681 = ORIENTED_EDGE ( 'NONE', *, *, #12199, .F. ) ;
#12682 = FACE_OUTER_BOUND ( 'NONE', #16845, .T. ) ;
#12683 = ORIENTED_EDGE ( 'NONE', *, *, #6741, .T. ) ;
#12684 = DIRECTION ( 'NONE',  ( -1.000000000000000000, -6.938893903907228378E-16, -0.000000000000000000 ) ) ;
#12685 = CARTESIAN_POINT ( 'NONE',  ( -26.89314795393037372, 18.00000000000000000, -11.55702759004479852 ) ) ;
#12686 = AXIS2_PLACEMENT_3D ( 'NONE', #179, #16802, #14066 ) ;
#12687 = EDGE_LOOP ( 'NONE', ( #630, #8927, #3544, #9760 ) ) ;
#12688 = CARTESIAN_POINT ( 'NONE',  ( 39.99999999999998579, -20.00000000000000000, 39.99999999999998579 ) ) ;
#12689 = AXIS2_PLACEMENT_3D ( 'NONE', #1488, #6880, #12368 ) ;
#12690 = DIRECTION ( 'NONE',  ( 0.000000000000000000, 0.000000000000000000, -1.000000000000000000 ) ) ;
#12691 = CARTESIAN_POINT ( 'NONE',  ( 16.25737266305939599, 136.9911583880083015, 7.117438641153603918 ) ) ;
#12692 = VERTEX_POINT ( 'NONE', #223 ) ;
#12693 = CONTEXT_DEPENDENT_SHAPE_REPRESENTATION ( #11947, #15052 ) ;
#12694 = CARTESIAN_POINT ( 'NONE',  ( 48.00000000000000711, 179.6227766016838245, 12.50000337241049309 ) ) ;
#12695 = CARTESIAN_POINT ( 'NONE',  ( 1.559999999999998943, 0.8660254037844428154, 1.500000000000001332 ) ) ;
#12696 = DIRECTION ( 'NONE',  ( -0.000000000000000000, 1.000000000000000000, 0.000000000000000000 ) ) ;
#12697 = CIRCLE ( 'NONE', #13546, 5.000000000000000888 ) ;
#12698 = DIRECTION ( 'NONE',  ( 0.000000000000000000, 0.000000000000000000, 1.000000000000000000 ) ) ;
#12699 = CARTESIAN_POINT ( 'NONE',  ( 17.54349574104648823, 125.4948194589026684, 4.999999999999997335 ) ) ;
#12700 = AXIS2_PLACEMENT_3D ( 'NONE', #4987, #5078, #8877 ) ;
#12701 = CARTESIAN_POINT ( 'NONE',  ( 22.50000000000000000, 196.6227766016838245, -35.00200000000000244 ) ) ;
#12702 = EDGE_CURVE ( 'NONE', #7474, #10091, #15735, .T. ) ;
#12703 = AXIS2_PLACEMENT_3D ( 'NONE', #1087, #14458, #13218 ) ;
#12704 = EDGE_CURVE ( 'NONE', #8718, #15454, #7969, .T. ) ;
#12705 = VERTEX_POINT ( 'NONE', #1156 ) ;
#12706 = DIRECTION ( 'NONE',  ( 1.000000000000000000, 0.000000000000000000, -0.000000000000000000 ) ) ;
#12707 = CARTESIAN_POINT ( 'NONE',  ( -95.00000000000000000, 171.6227766016838245, 0.000000000000000000 ) ) ;
#12708 = ORIENTED_EDGE ( 'NONE', *, *, #849, .T. ) ;
#12709 = FACE_BOUND ( 'NONE', #3877, .T. ) ;
#12710 = CARTESIAN_POINT ( 'NONE',  ( 22.93524650466160963, 29.84210526315773748, 4.999999999999999112 ) ) ;
#12711 = ORIENTED_EDGE ( 'NONE', *, *, #14772, .T. ) ;
#12712 = ORIENTED_EDGE ( 'NONE', *, *, #2726, .F. ) ;
#12713 = ORIENTED_EDGE ( 'NONE', *, *, #12704, .T. ) ;
#12714 = AXIS2_PLACEMENT_3D ( 'NONE', #10952, #13894, #4500 ) ;
#12715 = CARTESIAN_POINT ( 'NONE',  ( 9.414336857517209722, 132.5946763488762770, 12.41924194405873649 ) ) ;
#12716 = ADVANCED_FACE ( 'NONE', ( #10717 ), #15938, .F. ) ;
#12717 = AXIS2_PLACEMENT_3D ( 'NONE', #2493, #14716, #2592 ) ;
#12718 = ORIENTED_EDGE ( 'NONE', *, *, #446, .F. ) ;
#12719 = FACE_OUTER_BOUND ( 'NONE', #11291, .T. ) ;
#12720 = AXIS2_PLACEMENT_3D ( 'NONE', #11655, #7846, #17057 ) ;
#12721 = B_SPLINE_CURVE_WITH_KNOTS ( 'NONE', 3,
 ( #11812, #5006, #15807, #17218, #2434, #1113, #10571, #1471, #17312, #2621, #5453, #12183, #13333, #9249, #9600, #10669, #14826, #8007, #53, #2535, #3958, #10841, #16252, #16174, #11992, #3863, #5368, #14750, #13414, #13602, #4045, #10924, #13679, #17495, #10762, #1198, #8094, #4121, #9421, #17397, #9507, #8271 ),
 .UNSPECIFIED., .F., .F.,
 ( 4, 2, 2, 2, 2, 2, 2, 2, 2, 2, 2, 2, 2, 2, 2, 2, 2, 2, 2, 2, 4 ),
 ( 0.000000000000000000, 0.002338598163723741054, 0.002923247704654684340, 0.003507897245585628061, 0.004677196327447571446, 0.005846495409309514397, 0.006431144950240465057, 0.007015794491171416583, 0.008185093573033283207, 0.008769743113964226927, 0.009354392654895168913, 0.01052369173675701645, 0.01110834127768793762, 0.01169299081861886053, 0.01286228990048070633, 0.01403158898234255214, 0.01461623852327346637, 0.01520088806420438060, 0.01637018714606626457, 0.01753948622792815201, 0.01870878530979003598 ),
 .UNSPECIFIED. ) ;
#12722 = ORIENTED_EDGE ( 'NONE', *, *, #17322, .F. ) ;
#12723 = PRESENTATION_STYLE_ASSIGNMENT (( #5903 ) ) ;
#12724 = CARTESIAN_POINT ( 'NONE',  ( 49.99999999999998579, 187.6227766016837961, -10.00000337241049309 ) ) ;
#12725 = CARTESIAN_POINT ( 'NONE',  ( 14.23753691287610579, 127.5498911642838635, 8.870798623635511859 ) ) ;
#12726 = FACE_OUTER_BOUND ( 'NONE', #15831, .T. ) ;
#12727 = CARTESIAN_POINT ( 'NONE',  ( 49.99999999999998579, 183.6227766016837961, 3.071800142134975431 ) ) ;
#12728 = VERTEX_POINT ( 'NONE', #11860 ) ;
#12729 = CARTESIAN_POINT ( 'NONE',  ( 31.52965557968541432, 141.8580068101642269, 14.25043922611180136 ) ) ;
#12730 = VECTOR ( 'NONE', #13786, 1000.000000000000114 ) ;
#12731 = AXIS2_PLACEMENT_3D ( 'NONE', #2371, #7509, #6351 ) ;
#12732 = PLANE ( 'NONE',  #1681 ) ;
#12733 = CARTESIAN_POINT ( 'NONE',  ( 50.00000000000000000, 171.6227766016838245, 0.000000000000000000 ) ) ;
#12734 = VECTOR ( 'NONE', #9002, 1000.000000000000000 ) ;
#12735 = CARTESIAN_POINT ( 'NONE',  ( -10.16681828783789143, 30.62365918355438055, -14.67566226953583985 ) ) ;
#12736 = FACE_OUTER_BOUND ( 'NONE', #2670, .T. ) ;
#12737 = ADVANCED_FACE ( 'NONE', ( #15526 ), #3407, .T. ) ;
#12738 = ADVANCED_FACE ( 'NONE', ( #9205 ), #6561, .T. ) ;
#12739 = EDGE_CURVE ( 'NONE', #15148, #11161, #7881, .T. ) ;
#12740 = ORIENTED_EDGE ( 'NONE', *, *, #6132, .T. ) ;
#12741 = LINE ( 'NONE', #7240, #15456 ) ;
#12742 = AXIS2_PLACEMENT_3D ( 'NONE', #12576, #5762, #8155 ) ;
#12743 = CIRCLE ( 'NONE', #9330, 2.500000000000002220 ) ;
#12744 = EDGE_LOOP ( 'NONE', ( #7198, #14576 ) ) ;
#12745 = CARTESIAN_POINT ( 'NONE',  ( -24.99999999999999645, 120.0000000000000284, 0.000000000000000000 ) ) ;
#12746 = CIRCLE ( 'NONE', #11881, 2.500000000000002220 ) ;
#12747 = DIRECTION ( 'NONE',  ( -1.000000000000000000, 0.000000000000000000, -8.673617379884037937E-17 ) ) ;
#12748 = FACE_OUTER_BOUND ( 'NONE', #16361, .T. ) ;
#12749 = ORIENTED_EDGE ( 'NONE', *, *, #15325, .T. ) ;
#12750 = LINE ( 'NONE', #8838, #12077 ) ;
#12751 = DIRECTION ( 'NONE',  ( -1.000000000000000000, -0.000000000000000000, -0.000000000000000000 ) ) ;
#12752 = CARTESIAN_POINT ( 'NONE',  ( -82.24876160832761229, 201.0919203481101363, 14.85271610579512114 ) ) ;
#12753 = ORIENTED_EDGE ( 'NONE', *, *, #6786, .F. ) ;
#12754 = VECTOR ( 'NONE', #5625, 1000.000000000000000 ) ;
#12755 = EDGE_LOOP ( 'NONE', ( #7311, #15889, #6760, #6626 ) ) ;
#12756 = DIRECTION ( 'NONE',  ( 1.000000000000000000, 0.000000000000000000, 8.673617379884036705E-17 ) ) ;
#12757 = DIRECTION ( 'NONE',  ( 0.000000000000000000, 0.000000000000000000, 1.000000000000000000 ) ) ;
#12758 = ORIENTED_EDGE ( 'NONE', *, *, #13498, .T. ) ;
#12759 = DIRECTION ( 'NONE',  ( 0.000000000000000000, 1.000000000000000000, 2.312964634635742267E-15 ) ) ;
#12760 = CARTESIAN_POINT ( 'NONE',  ( 7.535032041484082121, 144.1839557648053187, -18.33333333253072794 ) ) ;
#12761 = ORIENTED_EDGE ( 'NONE', *, *, #16990, .F. ) ;
#12762 =( REPRESENTATION_RELATIONSHIP ('NONE','NONE', #9723, #690 ) REPRESENTATION_RELATIONSHIP_WITH_TRANSFORMATION ( #4815 )SHAPE_REPRESENTATION_RELATIONSHIP( ) );
#12763 = CARTESIAN_POINT ( 'NONE',  ( -27.99999999999998224, 10.00000000000000000, 28.00000000000000355 ) ) ;
#12764 = VECTOR ( 'NONE', #13395, 1000.000000000000000 ) ;
#12765 = CARTESIAN_POINT ( 'NONE',  ( 48.00000000000000711, 167.6227766016838814, 16.92820660268601429 ) ) ;
#12766 = CARTESIAN_POINT ( 'NONE',  ( -206.8260782938592683, 166.6501392256166127, -0.6181867824018475455 ) ) ;
#12767 = DIRECTION ( 'NONE',  ( 0.000000000000000000, 0.8660254037844413721, -0.4999999999999952816 ) ) ;
#12768 = CARTESIAN_POINT ( 'NONE',  ( -27.84784281930893357, 18.00000000000000000, 7.647248539284095870 ) ) ;
#12769 = LINE ( 'NONE', #11516, #13992 ) ;
#12770 = CARTESIAN_POINT ( 'NONE',  ( -15.00000000000002132, 100.0000000000000142, -4.999999999999999112 ) ) ;
#12771 = ORIENTED_EDGE ( 'NONE', *, *, #17138, .T. ) ;
#12772 = CARTESIAN_POINT ( 'NONE',  ( -157.2729844578908001, 171.6227766016838245, 0.000000000000000000 ) ) ;
#12773 = ORIENTED_EDGE ( 'NONE', *, *, #9160, .F. ) ;
#12774 = ADVANCED_FACE ( 'NONE', ( #11951 ), #17353, .F. ) ;
#12775 = CARTESIAN_POINT ( 'NONE',  ( -24.93725393319379435, 120.0000000000000284, 5.500000000000000000 ) ) ;
#12776 = DIRECTION ( 'NONE',  ( -1.000000000000000000, 0.000000000000000000, 0.000000000000000000 ) ) ;
#12777 = VERTEX_POINT ( 'NONE', #14207 ) ;
#12778 = CARTESIAN_POINT ( 'NONE',  ( 16.25302816831168329, 19.99999999999999645, 25.00000000000000000 ) ) ;
#12779 = CARTESIAN_POINT ( 'NONE',  ( 20.25331481973466907, 20.00000000000113687, 13.55662431013403868 ) ) ;
#12780 = CARTESIAN_POINT ( 'NONE',  ( 12.82285603306638144, 130.8395207603766153, 12.92896204370639524 ) ) ;
#12781 = VERTEX_POINT ( 'NONE', #2066 ) ;
#12782 = ITEM_DEFINED_TRANSFORMATION ( 'NONE', 'NONE', #9517,  #3583 ) ;
#12783 = CARTESIAN_POINT ( 'NONE',  ( -15.00000000000001421, 19.99999999999995737, -13.00000000000000000 ) ) ;
#12784 = DIRECTION ( 'NONE',  ( -1.000000000000000000, 0.000000000000000000, 0.000000000000000000 ) ) ;
#12785 = CARTESIAN_POINT ( 'NONE',  ( -80.38335849529188692, 191.6335950462331823, 26.24057872661396118 ) ) ;
#12786 = DIRECTION ( 'NONE',  ( -1.000000000000000000, -0.000000000000000000, -0.000000000000000000 ) ) ;
#12787 = DIRECTION ( 'NONE',  ( 1.000000000000000000, 0.000000000000000000, 0.000000000000000000 ) ) ;
#12788 = CARTESIAN_POINT ( 'NONE',  ( 27.99999999999998224, 9.999999999999998224, -13.00000000000000000 ) ) ;
#12789 = VERTEX_POINT ( 'NONE', #15609 ) ;
#12790 = SHAPE_REPRESENTATION ( '3-Stage Planetary Gearbox', ( #3583 ), #4757 ) ;
#12791 = LINE ( 'NONE', #9951, #13227 ) ;
#12792 = CARTESIAN_POINT ( 'NONE',  ( -16.40540729975244005, 20.00000000000000000, -23.03124090058168960 ) ) ;
#12793 = VERTEX_POINT ( 'NONE', #6468 ) ;
#12794 = EDGE_CURVE ( 'NONE', #12777, #668, #1894, .T. ) ;
#12795 = CARTESIAN_POINT ( 'NONE',  ( -68.00000000000000000, 154.3022685259950038, -9.999999999999900524 ) ) ;
#12796 = DIRECTION ( 'NONE',  ( -1.000000000000000000, 0.000000000000000000, 0.000000000000000000 ) ) ;
#12797 = VERTEX_POINT ( 'NONE', #659 ) ;
#12798 = ORIENTED_EDGE ( 'NONE', *, *, #12828, .T. ) ;
#12799 = EDGE_CURVE ( 'NONE', #17253, #14627, #3486, .T. ) ;
#12800 = VERTEX_POINT ( 'NONE', #17270 ) ;
#12801 = EDGE_CURVE ( 'NONE', #13379, #12251, #2584, .T. ) ;
#12802 = DIRECTION ( 'NONE',  ( -1.000000000000000000, 0.000000000000000000, 0.000000000000000000 ) ) ;
#12803 = ADVANCED_FACE ( 'NONE', ( #12867 ), #14279, .T. ) ;
#12804 = VERTEX_POINT ( 'NONE', #10531 ) ;
#12805 =( LENGTH_UNIT ( ) NAMED_UNIT ( * ) SI_UNIT ( .MILLI., .METRE. ) );
#12806 = FACE_OUTER_BOUND ( 'NONE', #15845, .T. ) ;
#12807 = LINE ( 'NONE', #11300, #11183 ) ;
#12808 = CARTESIAN_POINT ( 'NONE',  ( -157.2729844578908001, 171.6227766016838245, 0.000000000000000000 ) ) ;
#12809 = CARTESIAN_POINT ( 'NONE',  ( 35.27494917608787972, 141.2912748254776147, -13.00000000000000000 ) ) ;
#12810 = ORIENTED_EDGE ( 'NONE', *, *, #9529, .T. ) ;
#12811 = DIRECTION ( 'NONE',  ( 0.000000000000000000, 0.000000000000000000, 1.000000000000000000 ) ) ;
#12812 = DIRECTION ( 'NONE',  ( -1.000000000000000000, 0.000000000000000000, 0.000000000000000000 ) ) ;
#12813 = CARTESIAN_POINT ( 'NONE',  ( -24.93725393319378725, 100.0000000000000142, 5.500000000000000000 ) ) ;
#12814 = FACE_OUTER_BOUND ( 'NONE', #17306, .T. ) ;
#12815 = CARTESIAN_POINT ( 'NONE',  ( 49.99999999999998579, 167.6227766016838814, 16.92820660268601429 ) ) ;
#12816 = PRODUCT_DEFINITION_SHAPE ( 'NONE', 'NONE',  #17529 ) ;
#12817 = CARTESIAN_POINT ( 'NONE',  ( 225.0000000000000000, 89.99999999999997158, -15.00000000000000000 ) ) ;
#12818 = ORIENTED_EDGE ( 'NONE', *, *, #10012, .T. ) ;
#12819 = DIRECTION ( 'NONE',  ( 0.9961946980917464334, -0.04357787137382450326, 0.07547908730516456055 ) ) ;
#12820 = ORIENTED_EDGE ( 'NONE', *, *, #1362, .F. ) ;
#12821 = CARTESIAN_POINT ( 'NONE',  ( 20.99355996702781724, 139.9415946336124534, 14.89340340269096785 ) ) ;
#12822 = LINE ( 'NONE', #16989, #3366 ) ;
#12823 = CYLINDRICAL_SURFACE ( 'NONE', #1816, 2.500000000000000444 ) ;
#12824 = ORIENTED_EDGE ( 'NONE', *, *, #9891, .T. ) ;
#12825 = CARTESIAN_POINT ( 'NONE',  ( 22.93524650466160963, 29.84210526315773748, 15.00000000000000000 ) ) ;
#12826 = DIRECTION ( 'NONE',  ( 0.000000000000000000, 0.000000000000000000, -1.000000000000000000 ) ) ;
#12827 = EDGE_CURVE ( 'NONE', #17297, #846, #1042, .T. ) ;
#12828 = EDGE_CURVE ( 'NONE', #8077, #12595, #7273, .T. ) ;
#12829 = CARTESIAN_POINT ( 'NONE',  ( -997.5739745962155212, 0.000000000000000000, 0.000000000000000000 ) ) ;
#12830 = CARTESIAN_POINT ( 'NONE',  ( 25.93937429209274015, 201.0559264674919007, -18.94433901724532276 ) ) ;
#12831 = EDGE_LOOP ( 'NONE', ( #12488, #10813, #6484, #16071 ) ) ;
#12832 = ORIENTED_EDGE ( 'NONE', *, *, #1988, .T. ) ;
#12833 = CARTESIAN_POINT ( 'NONE',  ( 19.38030756396766563, 20.00000000000112621, -14.02844645440659654 ) ) ;
#12834 = CARTESIAN_POINT ( 'NONE',  ( 16.87754908408646415, 142.8876428028120813, -16.22928829806427942 ) ) ;
#12835 = ORIENTED_EDGE ( 'NONE', *, *, #7811, .T. ) ;
#12836 = FACE_OUTER_BOUND ( 'NONE', #402, .T. ) ;
#12837 = LINE ( 'NONE', #17081, #5254 ) ;
#12838 = ORIENTED_EDGE ( 'NONE', *, *, #1221, .F. ) ;
#12839 = DIRECTION ( 'NONE',  ( -1.000000000000000000, 0.000000000000000000, 0.000000000000000000 ) ) ;
#12840 = UNCERTAINTY_MEASURE_WITH_UNIT (LENGTH_MEASURE( 1.000000000000000082E-05 ), #15910, 'distance_accuracy_value', 'NONE');
#12841 = DIRECTION ( 'NONE',  ( -1.000000000000000000, 0.000000000000000000, 0.000000000000000000 ) ) ;
#12842 = AXIS2_PLACEMENT_3D ( 'NONE', #10417, #13087, #2029 ) ;
#12843 = CARTESIAN_POINT ( 'NONE',  ( 17.00000000000000000, 154.3022685259950038, 9.999999999999900524 ) ) ;
#12844 = CARTESIAN_POINT ( 'NONE',  ( -9.480043248727735516, 17.99999999999769784, 11.96743332394513715 ) ) ;
#12845 = ADVANCED_FACE ( 'NONE', ( #6647 ), #15749, .T. ) ;
#12846 = ADVANCED_FACE ( 'NONE', ( #6054 ), #7551, .T. ) ;
#12847 = DIRECTION ( 'NONE',  ( 0.000000000000000000, 0.5000000000000011102, -0.8660254037844379305 ) ) ;
#12848 = EDGE_CURVE ( 'NONE', #2606, #15093, #8401, .T. ) ;
#12849 = EDGE_CURVE ( 'NONE', #4227, #6176, #11136, .T. ) ;
#12850 = CARTESIAN_POINT ( 'NONE',  ( 35.34529388524494209, 143.8751093726684758, -21.33821933965574402 ) ) ;
#12851 = EDGE_LOOP ( 'NONE', ( #16186, #5232, #7301, #3494 ) ) ;
#12852 = DIRECTION ( 'NONE',  ( 0.000000000000000000, -0.8660254037844388186, 0.4999999999999996114 ) ) ;
#12853 = VERTEX_POINT ( 'NONE', #13553 ) ;
#12854 = CARTESIAN_POINT ( 'NONE',  ( -75.00000000000000000, 196.6227766016838245, -35.00200000000000244 ) ) ;
#12855 = DIRECTION ( 'NONE',  ( 1.000000000000000000, 0.000000000000000000, 0.000000000000000000 ) ) ;
#12856 = ORIENTED_EDGE ( 'NONE', *, *, #7910, .T. ) ;
#12857 = DIRECTION ( 'NONE',  ( 0.000000000000000000, 0.000000000000000000, 1.000000000000000000 ) ) ;
#12858 = VECTOR ( 'NONE', #16153, 1000.000000000000000 ) ;
#12859 = PRESENTATION_LAYER_ASSIGNMENT (  '', '', ( #15396 ) ) ;
#12860 = CARTESIAN_POINT ( 'NONE',  ( -73.34456489498955989, 200.1146145092350821, -16.67123533649924383 ) ) ;
#12861 = CYLINDRICAL_SURFACE ( 'NONE', #13519, 2.500000000000000444 ) ;
#12862 = ORIENTED_EDGE ( 'NONE', *, *, #25, .F. ) ;
#12863 = EDGE_CURVE ( 'NONE', #2141, #2623, #9724, .T. ) ;
#12864 = DIRECTION ( 'NONE',  ( 0.000000000000000000, 0.000000000000000000, 1.000000000000000000 ) ) ;
#12865 = CARTESIAN_POINT ( 'NONE',  ( -84.06590298985813092, 193.6946896392257997, 24.53450862945289401 ) ) ;
#12866 = CARTESIAN_POINT ( 'NONE',  ( -73.00000000000001421, 171.6227766016838245, 5.000000000000007994 ) ) ;
#12867 = FACE_OUTER_BOUND ( 'NONE', #16398, .T. ) ;
#12868 = LINE ( 'NONE', #1901, #17369 ) ;
#12869 = AXIS2_PLACEMENT_3D ( 'NONE', #6620, #950, #6440 ) ;
#12870 = ORIENTED_EDGE ( 'NONE', *, *, #937, .T. ) ;
#12871 = DIRECTION ( 'NONE',  ( 0.000000000000000000, 0.000000000000000000, 1.000000000000000000 ) ) ;
#12873 = CARTESIAN_POINT ( 'NONE',  ( -19.79962810613638169, 20.00000000000000355, -20.97942696524415851 ) ) ;
#12872 = VECTOR ( 'NONE', #2903, 1000.000000000000000 ) ;
#12874 = ORIENTED_EDGE ( 'NONE', *, *, #6721, .T. ) ;
#12875 = DIRECTION ( 'NONE',  ( 1.000000000000000000, -0.000000000000000000, -0.000000000000000000 ) ) ;
#12876 = AXIS2_PLACEMENT_3D ( 'NONE', #15461, #11302, #11206 ) ;
#12877 = DIRECTION ( 'NONE',  ( -0.000000000000000000, -0.000000000000000000, 1.000000000000000000 ) ) ;
#12878 = VERTEX_POINT ( 'NONE', #3003 ) ;
#12879 = EDGE_LOOP ( 'NONE', ( #3917, #13662, #6215, #610, #16464 ) ) ;
#12880 = ORIENTED_EDGE ( 'NONE', *, *, #15485, .T. ) ;
#12881 = ORIENTED_EDGE ( 'NONE', *, *, #12034, .T. ) ;
#12882 = PRESENTATION_STYLE_ASSIGNMENT (( #13883 ) ) ;
#12883 = PRESENTATION_LAYER_ASSIGNMENT (  '', '', ( #2413 ) ) ;
#12884 = ORIENTED_EDGE ( 'NONE', *, *, #1233, .T. ) ;
#12885 =( NAMED_UNIT ( * ) SI_UNIT ( $, .STERADIAN. ) SOLID_ANGLE_UNIT ( ) );
#12886 = EDGE_CURVE ( 'NONE', #7241, #5755, #2660, .T. ) ;
#12887 = DIRECTION ( 'NONE',  ( -1.000000000000000000, -0.000000000000000000, 0.000000000000000000 ) ) ;
#12888 = CIRCLE ( 'NONE', #6946, 2.499999999999998668 ) ;
#12889 = EDGE_CURVE ( 'NONE', #14544, #5702, #6737, .T. ) ;
#12890 = LINE ( 'NONE', #14144, #13157 ) ;
#12891 =( BOUNDED_CURVE ( )  B_SPLINE_CURVE ( 3, ( #7213, #16444, #4307, #6871 ),
 .UNSPECIFIED., .F., .F. ) 
 B_SPLINE_CURVE_WITH_KNOTS ( ( 4, 4 ),
 ( 1.570796326794899000, 3.141592653589791340 ),
 .UNSPECIFIED. ) 
 CURVE ( )  GEOMETRIC_REPRESENTATION_ITEM ( )  RATIONAL_B_SPLINE_CURVE ( ( 1.000000000000000000, 0.8047378541243659367, 0.8047378541243659367, 1.000000000000000000 ) ) 
 REPRESENTATION_ITEM ( '' )  );
#12892 = VECTOR ( 'NONE', #715, 1000.000000000000000 ) ;
#12893 = CARTESIAN_POINT ( 'NONE',  ( 49.99999999999998579, 167.6227766016838814, 19.42820660268601074 ) ) ;
#12894 = LINE ( 'NONE', #15895, #5524 ) ;
#12895 = VERTEX_POINT ( 'NONE', #5412 ) ;
#12896 = FACE_OUTER_BOUND ( 'NONE', #12002, .T. ) ;
#12897 = DIRECTION ( 'NONE',  ( 0.000000000000000000, 0.000000000000000000, 1.000000000000000000 ) ) ;
#12898 = DIRECTION ( 'NONE',  ( -0.000000000000000000, -0.000000000000000000, -1.000000000000000000 ) ) ;
#12899 = ADVANCED_FACE ( 'NONE', ( #1687 ), #13818, .F. ) ;
#12900 = CARTESIAN_POINT ( 'NONE',  ( -16.58710929330769090, 31.97525413706907216, -10.34574908881256050 ) ) ;
#12901 = DIRECTION ( 'NONE',  ( 0.000000000000000000, 0.000000000000000000, 1.000000000000000000 ) ) ;
#12902 = EDGE_CURVE ( 'NONE', #7137, #13658, #12219, .T. ) ;
#12903 = CIRCLE ( 'NONE', #5546, 9.999999999999998224 ) ;
#12904 = VECTOR ( 'NONE', #9324, 1000.000000000000000 ) ;
#12905 = CARTESIAN_POINT ( 'NONE',  ( -27.99999999999998224, 10.00000000000000000, 35.00200000000000244 ) ) ;
#12906 = ORIENTED_EDGE ( 'NONE', *, *, #10061, .T. ) ;
#12907 = CARTESIAN_POINT ( 'NONE',  ( -3.000000000000000888, 204.6227766016838245, -2.020667218593133100E-15 ) ) ;
#12908 = ADVANCED_BREP_SHAPE_REPRESENTATION ( '', ( #11096, #11475, #5484, #3583 ), #12675 ) ;
#12909 = ORIENTED_EDGE ( 'NONE', *, *, #4926, .T. ) ;
#12910 = CARTESIAN_POINT ( 'NONE',  ( 14.58358448378887928, 141.6717822189192191, 18.11319387340528309 ) ) ;
#12911 = CIRCLE ( 'NONE', #5280, 7.500000000000003553 ) ;
#12912 = DIRECTION ( 'NONE',  ( -0.000000000000000000, -0.000000000000000000, 1.000000000000000000 ) ) ;
#12913 = DIRECTION ( 'NONE',  ( 8.673617379884037937E-17, 0.000000000000000000, 1.000000000000000000 ) ) ;
#12914 = TOROIDAL_SURFACE ( 'NONE', #188, 2.699999999999999289, 0.2000000000000000111 ) ;
#12915 = ORIENTED_EDGE ( 'NONE', *, *, #14451, .F. ) ;
#12916 = DIRECTION ( 'NONE',  ( -1.000000000000000000, -0.000000000000000000, -0.000000000000000000 ) ) ;
#12917 = DIRECTION ( 'NONE',  ( 0.000000000000000000, 1.000000000000000000, 0.000000000000000000 ) ) ;
#12918 = DIRECTION ( 'NONE',  ( 0.000000000000000000, 0.000000000000000000, 1.000000000000000000 ) ) ;
#12919 = CARTESIAN_POINT ( 'NONE',  ( 32.41901710885975518, 202.1180966153993097, -17.17743398583138870 ) ) ;
#12920 = EDGE_CURVE ( 'NONE', #4758, #13658, #8680, .T. ) ;
#12921 = ORIENTED_EDGE ( 'NONE', *, *, #15495, .F. ) ;
#12922 = EDGE_LOOP ( 'NONE', ( #8872, #3469, #11590, #1636, #17130, #2925, #16665 ) ) ;
#12923 = CARTESIAN_POINT ( 'NONE',  ( 18.16394926501914497, 19.99999999999999645, -14.51477632729204537 ) ) ;
#12924 = VECTOR ( 'NONE', #17431, 1000.000000000000000 ) ;
#12925 = DIRECTION ( 'NONE',  ( -1.000000000000000000, 0.000000000000000000, 0.000000000000000000 ) ) ;
#12926 = AXIS2_PLACEMENT_3D ( 'NONE', #9817, #4777, #3267 ) ;
#12927 = ORIENTED_EDGE ( 'NONE', *, *, #3820, .T. ) ;
#12928 = COLOUR_RGB ( '', 0.66274510, 0.83137255, 0.94901961) ;
#12929 = CARTESIAN_POINT ( 'NONE',  ( 30.00000000000001066, 146.6227766016838245, 35.00200000000000244 ) ) ;
#12930 = AXIS2_PLACEMENT_3D ( 'NONE', #3878, #14491, #6615 ) ;
#12931 = DIRECTION ( 'NONE',  ( 0.000000000000000000, 0.000000000000000000, 1.000000000000000000 ) ) ;
#12932 = ORIENTED_EDGE ( 'NONE', *, *, #11421, .T. ) ;
#12933 = ADVANCED_FACE ( 'NONE', ( #1427 ), #4079, .T. ) ;
#12934 = CARTESIAN_POINT ( 'NONE',  ( 36.42104199761076444, 200.5259344270105260, -15.94638436093397083 ) ) ;
#12935 = CARTESIAN_POINT ( 'NONE',  ( -68.00000000000000000, 171.6227766016838245, 0.000000000000000000 ) ) ;
#12936 = CARTESIAN_POINT ( 'NONE',  ( -50.00000000000000000, 171.6227766016838245, 24.99999999999999289 ) ) ;
#12937 = CARTESIAN_POINT ( 'NONE',  ( -10.50630597522742171, 31.01369813559846378, 12.50559288035636563 ) ) ;
#12938 = VECTOR ( 'NONE', #9888, 1000.000000000000000 ) ;
#12939 = CARTESIAN_POINT ( 'NONE',  ( -23.00000000000001421, 122.0000000000000284, 4.999999999999999112 ) ) ;
#12940 = AXIS2_PLACEMENT_3D ( 'NONE', #11008, #2950, #3214 ) ;
#12941 = AXIS2_PLACEMENT_3D ( 'NONE', #4637, #1978, #7382 ) ;
#12942 = CARTESIAN_POINT ( 'NONE',  ( 36.00000000000002132, 146.6227766016838245, -24.49489742783179125 ) ) ;
#12943 = EDGE_LOOP ( 'NONE', ( #13079, #5398 ) ) ;
#12944 = CARTESIAN_POINT ( 'NONE',  ( -70.00000000000000000, 154.3022685259950038, -9.999999999999900524 ) ) ;
#12945 = ORIENTED_EDGE ( 'NONE', *, *, #17363, .F. ) ;
#12946 = CARTESIAN_POINT ( 'NONE',  ( 225.0000000000000000, 89.99999999999997158, 0.000000000000000000 ) ) ;
#12947 = DIRECTION ( 'NONE',  ( 1.000000000000000000, 0.000000000000000000, 0.000000000000000000 ) ) ;
#12948 = ORIENTED_EDGE ( 'NONE', *, *, #9211, .T. ) ;
#12949 = CARTESIAN_POINT ( 'NONE',  ( 30.81698523721487604, 20.00000000000000355, 17.17210857557096659 ) ) ;
#12950 = EDGE_CURVE ( 'NONE', #7206, #15700, #10660, .T. ) ;
#12951 = EDGE_CURVE ( 'NONE', #7374, #16329, #6138, .T. ) ;
#12952 = CIRCLE ( 'NONE', #14364, 2.499999999999998668 ) ;
#12953 = CARTESIAN_POINT ( 'NONE',  ( 23.92105171931311958, 29.88144160311327724, 9.435928464502936208 ) ) ;
#12954 = EDGE_CURVE ( 'NONE', #15922, #4370, #17454, .T. ) ;
#12955 = AXIS2_PLACEMENT_3D ( 'NONE', #14701, #13455, #4 ) ;
#12956 = ORIENTED_EDGE ( 'NONE', *, *, #11712, .F. ) ;
#12957 = DIRECTION ( 'NONE',  ( 1.000000000000000000, 0.000000000000000000, 0.000000000000000000 ) ) ;
#12958 = CYLINDRICAL_SURFACE ( 'NONE', #10425, 10.00000000000000000 ) ;
#12959 = CARTESIAN_POINT ( 'NONE',  ( -15.37994105483213758, 31.72997864396344525, -11.82123051499886479 ) ) ;
#12960 = LINE ( 'NONE', #11449, #15656 ) ;
#12961 = VERTEX_POINT ( 'NONE', #2751 ) ;
#12962 = CARTESIAN_POINT ( 'NONE',  ( -95.00000000000000000, 201.6227766016838245, -1.836970198721029589E-15 ) ) ;
#12963 = AXIS2_PLACEMENT_3D ( 'NONE', #12772, #454, #1883 ) ;
#12964 = CYLINDRICAL_SURFACE ( 'NONE', #5686, 6.000000000000008882 ) ;
#12965 = ORIENTED_EDGE ( 'NONE', *, *, #13939, .F. ) ;
#12966 = CARTESIAN_POINT ( 'NONE',  ( -207.9324504923922348, 175.6261042361158786, -3.902623366482125267 ) ) ;
#12967 = AXIS2_PLACEMENT_3D ( 'NONE', #8208, #9618, #1400 ) ;
#12968 = DIRECTION ( 'NONE',  ( -1.000000000000000000, 0.000000000000000000, 0.000000000000000000 ) ) ;
#12969 = ORIENTED_EDGE ( 'NONE', *, *, #1129, .F. ) ;
#12970 = VERTEX_POINT ( 'NONE', #8141 ) ;
#12971 = ORIENTED_EDGE ( 'NONE', *, *, #3347, .T. ) ;
#12972 = LINE ( 'NONE', #11635, #6156 ) ;
#12973 = VECTOR ( 'NONE', #14171, 1000.000000000000000 ) ;
#12974 = ORIENTED_EDGE ( 'NONE', *, *, #11030, .T. ) ;
#12975 = DIRECTION ( 'NONE',  ( 1.000000000000000000, 0.000000000000000000, 0.000000000000000000 ) ) ;
#12976 = AXIS2_PLACEMENT_3D ( 'NONE', #3413, #2074, #4738 ) ;
#12977 = FACE_OUTER_BOUND ( 'NONE', #15603, .T. ) ;
#12978 = AXIS2_PLACEMENT_3D ( 'NONE', #9069, #14395, #2533 ) ;
#12979 = LINE ( 'NONE', #10228, #10042 ) ;
#12980 = CARTESIAN_POINT ( 'NONE',  ( 39.99999999999998579, -20.00000000000000000, 39.99999999999998579 ) ) ;
#12981 = CARTESIAN_POINT ( 'NONE',  ( 30.80964797964692536, 18.00000000000000000, 17.18170494867161224 ) ) ;
#12982 = FACE_OUTER_BOUND ( 'NONE', #1628, .T. ) ;
#12983 = EDGE_LOOP ( 'NONE', ( #2247, #3555 ) ) ;
#12984 = DIRECTION ( 'NONE',  ( 1.000000000000000000, 0.000000000000000000, 0.000000000000000000 ) ) ;
#12985 = DIRECTION ( 'NONE',  ( 1.000000000000000000, 0.000000000000000000, 0.000000000000000000 ) ) ;
#12986 = CARTESIAN_POINT ( 'NONE',  ( 1.559999999999998943, 1.732050807568885631, 0.000000000000000000 ) ) ;
#12987 = CARTESIAN_POINT ( 'NONE',  ( -15.09561842307909707, 19.99999999999307931, -7.342182892333040556 ) ) ;
#12988 = DIRECTION ( 'NONE',  ( 1.000000000000000000, 0.000000000000000000, 0.000000000000000000 ) ) ;
#12989 = CONICAL_SURFACE ( 'NONE', #9023, 2.500000000000002220, 1.029744260000002631 ) ;
#12990 = AXIS2_PLACEMENT_3D ( 'NONE', #979, #17018, #15945 ) ;
#12991 = ADVANCED_FACE ( 'NONE', ( #1504 ), #8, .F. ) ;
#12992 = AXIS2_PLACEMENT_3D ( 'NONE', #5781, #12432, #12690 ) ;
#12993 = CARTESIAN_POINT ( 'NONE',  ( -95.00000000000000000, 171.6227766016838245, -30.00000000000000000 ) ) ;
#12994 = ORIENTED_EDGE ( 'NONE', *, *, #4717, .F. ) ;
#12995 = DIRECTION ( 'NONE',  ( -1.000000000000000000, -0.000000000000000000, -0.000000000000000000 ) ) ;
#12996 = DIRECTION ( 'NONE',  ( 0.9961946980917464334, 0.08715574274764831264, 0.000000000000000000 ) ) ;
#12997 = VERTEX_POINT ( 'NONE', #8052 ) ;
#12998 =( NAMED_UNIT ( * ) PLANE_ANGLE_UNIT ( ) SI_UNIT ( $, .RADIAN. ) );
#12999 = CARTESIAN_POINT ( 'NONE',  ( 6.134011831684053284, 142.5209969267753820, 19.44444444444444642 ) ) ;
#13000 = EDGE_CURVE ( 'NONE', #1173, #2136, #10969, .T. ) ;
#13001 = CIRCLE ( 'NONE', #13859, 2.500000000000000000 ) ;
#13002 = LINE ( 'NONE', #4934, #15790 ) ;
#13003 = AXIS2_PLACEMENT_3D ( 'NONE', #2586, #9463, #13464 ) ;
#13004 = CIRCLE ( 'NONE', #3, 23.61711149033412127 ) ;
#13005 = LINE ( 'NONE', #9005, #1244 ) ;
#13006 = ORIENTED_EDGE ( 'NONE', *, *, #15704, .F. ) ;
#13007 = LINE ( 'NONE', #7951, #1631 ) ;
#13008 = DIRECTION ( 'NONE',  ( 1.000000000000000000, 0.000000000000000000, 0.000000000000000000 ) ) ;
#13009 = CARTESIAN_POINT ( 'NONE',  ( -32.99999999999998579, 10.00000000000000000, 0.000000000000000000 ) ) ;
#13010 = DIRECTION ( 'NONE',  ( -1.000000000000000000, 0.000000000000000000, -8.673617379884037937E-17 ) ) ;
#13011 = ORIENTED_EDGE ( 'NONE', *, *, #10246, .T. ) ;
#13012 = ORIENTED_EDGE ( 'NONE', *, *, #4441, .F. ) ;
#13013 = EDGE_CURVE ( 'NONE', #8812, #6709, #4430, .T. ) ;
#13014 = CARTESIAN_POINT ( 'NONE',  ( 29.53214135918837968, 19.99999999999999645, -18.68621337608103516 ) ) ;
#13015 = AXIS2_PLACEMENT_3D ( 'NONE', #15206, #14068, #3083 ) ;
#13016 = CIRCLE ( 'NONE', #10189, 20.00000000000000355 ) ;
#13017 = CARTESIAN_POINT ( 'NONE',  ( 11.58137902169779920, 142.1604892273610687, -18.89461017025931966 ) ) ;
#13018 = ORIENTED_EDGE ( 'NONE', *, *, #16538, .F. ) ;
#13019 = DIRECTION ( 'NONE',  ( 0.000000000000000000, 0.000000000000000000, 1.000000000000000000 ) ) ;
#13020 = AXIS2_PLACEMENT_3D ( 'NONE', #3161, #8554, #4582 ) ;
#13021 = DIRECTION ( 'NONE',  ( -0.000000000000000000, -0.000000000000000000, -1.000000000000000000 ) ) ;
#13022 = ADVANCED_FACE ( 'NONE', ( #6990 ), #5859, .T. ) ;
#13023 = EDGE_LOOP ( 'NONE', ( #14448, #3974, #3623, #9994 ) ) ;
#13024 = CARTESIAN_POINT ( 'NONE',  ( -80.00000000000002842, 146.6227766016838245, -13.00000000000000000 ) ) ;
#13025 = EDGE_CURVE ( 'NONE', #7898, #16968, #3023, .T. ) ;
#13026 = EDGE_CURVE ( 'NONE', #17370, #11034, #9905, .T. ) ;
#13027 = DIRECTION ( 'NONE',  ( -0.000000000000000000, -0.000000000000000000, -1.000000000000000000 ) ) ;
#13028 = CARTESIAN_POINT ( 'NONE',  ( 27.99999999999998224, 9.999999999999998224, -35.00000000000000000 ) ) ;
#13029 = CARTESIAN_POINT ( 'NONE',  ( -11.82448321327245466, 31.42688426858654438, 11.97038274549936254 ) ) ;
#13030 = CARTESIAN_POINT ( 'NONE',  ( -50.00000000000000000, 143.0439382767972631, -16.49999999999984013 ) ) ;
#13031 = AXIS2_PLACEMENT_3D ( 'NONE', #10020, #16773, #383 ) ;
#13032 = CARTESIAN_POINT ( 'NONE',  ( 29.47106614592656015, 140.6403763931701576, -16.28177936134992621 ) ) ;
#13033 = ORIENTED_EDGE ( 'NONE', *, *, #12376, .F. ) ;
#13034 = DIRECTION ( 'NONE',  ( 0.8571673013836867971, 1.049727191973306626E-16, -0.5150380737757237481 ) ) ;
#13035 = EDGE_CURVE ( 'NONE', #9392, #11112, #4605, .T. ) ;
#13036 = ORIENTED_EDGE ( 'NONE', *, *, #12199, .T. ) ;
#13037 = CARTESIAN_POINT ( 'NONE',  ( -24.93725393319378725, 100.0000000000000142, 5.500000000000000000 ) ) ;
#13038 = DIRECTION ( 'NONE',  ( 1.000000000000000000, 1.156482317317868274E-16, 0.000000000000000000 ) ) ;
#13039 = EDGE_LOOP ( 'NONE', ( #13252, #17005, #7257, #15571, #3733 ) ) ;
#13040 = CARTESIAN_POINT ( 'NONE',  ( 25.51458778375578973, 19.99999999999999289, 21.98440010584615578 ) ) ;
#13041 = DIRECTION ( 'NONE',  ( -1.000000000000000000, 0.000000000000000000, 0.000000000000000000 ) ) ;
#13042 = VECTOR ( 'NONE', #8869, 1000.000000000000000 ) ;
#13043 = CARTESIAN_POINT ( 'NONE',  ( 22.23358001889399205, 29.90326853444953059, 11.84310668804517697 ) ) ;
#13044 = EDGE_LOOP ( 'NONE', ( #16235, #10500 ) ) ;
#13045 = CARTESIAN_POINT ( 'NONE',  ( -208.1430079281944074, 172.4097984991905150, 5.932774073184737595 ) ) ;
#13046 = CARTESIAN_POINT ( 'NONE',  ( 49.99999999999998579, 167.6227766016838530, 3.071800142134975431 ) ) ;
#13047 = CARTESIAN_POINT ( 'NONE',  ( 30.00000000000001066, 146.6227766016838245, -16.00000000000000000 ) ) ;
#13048 = CARTESIAN_POINT ( 'NONE',  ( -25.16839285024616402, 18.00000000000000000, -15.12082343620105540 ) ) ;
#13049 = EDGE_LOOP ( 'NONE', ( #16148, #17171, #14876, #17036 ) ) ;
#13050 = FACE_OUTER_BOUND ( 'NONE', #15278, .T. ) ;
#13051 = CIRCLE ( 'NONE', #2305, 2.500000000000002220 ) ;
#13052 = ADVANCED_FACE ( 'NONE', ( #16815, #6014 ), #3449, .F. ) ;
#13053 = EDGE_CURVE ( 'NONE', #14777, #15022, #16736, .T. ) ;
#13054 = EDGE_CURVE ( 'NONE', #9101, #3454, #14081, .T. ) ;
#13055 = ORIENTED_EDGE ( 'NONE', *, *, #14370, .F. ) ;
#13056 = CARTESIAN_POINT ( 'NONE',  ( 28.43487082456423209, 190.8261496651128937, -29.26147795858665290 ) ) ;
#13057 = CARTESIAN_POINT ( 'NONE',  ( -40.00000000000000711, 0.000000000000000000, 0.000000000000000000 ) ) ;
#13058 = ORIENTED_EDGE ( 'NONE', *, *, #11728, .T. ) ;
#13059 = ORIENTED_EDGE ( 'NONE', *, *, #16978, .T. ) ;
#13060 = VERTEX_POINT ( 'NONE', #2031 ) ;
#13061 = CARTESIAN_POINT ( 'NONE',  ( -85.45515645957152628, 151.7936747764227334, -26.38258506112510560 ) ) ;
#13062 = ORIENTED_EDGE ( 'NONE', *, *, #12702, .F. ) ;
#13063 = CARTESIAN_POINT ( 'NONE',  ( 0.000000000000000000, 0.000000000000000000, 0.000000000000000000 ) ) ;
#13064 = CARTESIAN_POINT ( 'NONE',  ( -12.54777316999452275, 31.64944667534048861, 11.54374194473465920 ) ) ;
#13065 = CARTESIAN_POINT ( 'NONE',  ( -18.25212770525996930, 32.30769230769229949, 5.349717987761776428 ) ) ;
#13066 = CARTESIAN_POINT ( 'NONE',  ( 24.85999067142302010, 149.7234947166294035, -27.30319596934541693 ) ) ;
#13067 = CARTESIAN_POINT ( 'NONE',  ( 15.00000000000000000, 154.3022685259950038, -9.999999999999900524 ) ) ;
#13068 = CARTESIAN_POINT ( 'NONE',  ( -68.00000000000000000, 171.6227766016838245, 0.000000000000000000 ) ) ;
#13069 = ORIENTED_EDGE ( 'NONE', *, *, #9455, .F. ) ;
#13070 = DIRECTION ( 'NONE',  ( -1.000000000000000000, 0.000000000000000000, 0.000000000000000000 ) ) ;
#13071 = DIRECTION ( 'NONE',  ( 0.000000000000000000, -1.000000000000000000, 0.000000000000000000 ) ) ;
#13072 = EDGE_CURVE ( 'NONE', #11521, #8796, #2178, .T. ) ;
#13073 = EDGE_CURVE ( 'NONE', #16820, #9959, #12750, .T. ) ;
#13074 = CYLINDRICAL_SURFACE ( 'NONE', #12172, 2.499999999999998668 ) ;
#13075 = CARTESIAN_POINT ( 'NONE',  ( -18.25212770525392614, 32.30769230766699707, -5.660855707253096725 ) ) ;
#13076 = EDGE_LOOP ( 'NONE', ( #7993, #54 ) ) ;
#13077 = DIRECTION ( 'NONE',  ( -0.000000000000000000, -0.000000000000000000, 1.000000000000000000 ) ) ;
#13078 = CARTESIAN_POINT ( 'NONE',  ( 28.25663979599552178, 201.3127097690254175, 14.40604465277983159 ) ) ;
#13079 = ORIENTED_EDGE ( 'NONE', *, *, #16165, .F. ) ;
#13080 = PLANE ( 'NONE',  #14949 ) ;
#13081 = VERTEX_POINT ( 'NONE', #4687 ) ;
#13082 =( NAMED_UNIT ( * ) SI_UNIT ( $, .STERADIAN. ) SOLID_ANGLE_UNIT ( ) );
#13083 = CARTESIAN_POINT ( 'NONE',  ( -78.86956020503002662, 141.7478424248370175, 14.01801864773821649 ) ) ;
#13084 = CARTESIAN_POINT ( 'NONE',  ( 15.97577464858015617, 18.00000000000228084, -12.97048270532338243 ) ) ;
#13085 = CARTESIAN_POINT ( 'NONE',  ( -81.29609393525485928, 140.7594520581393738, -16.50672721711051238 ) ) ;
#13086 = EDGE_CURVE ( 'NONE', #11927, #17386, #3362, .T. ) ;
#13087 = DIRECTION ( 'NONE',  ( 1.000000000000000000, 0.000000000000000000, -0.000000000000000000 ) ) ;
#13088 = ORIENTED_EDGE ( 'NONE', *, *, #9652, .T. ) ;
#13089 = DIRECTION ( 'NONE',  ( -1.000000000000000000, 0.000000000000000000, -8.673617379884037937E-17 ) ) ;
#13090 = DIRECTION ( 'NONE',  ( 1.000000000000000000, 0.000000000000000000, 0.000000000000000000 ) ) ;
#13091 = DIRECTION ( 'NONE',  ( 0.000000000000000000, 0.000000000000000000, 1.000000000000000000 ) ) ;
#13092 = CARTESIAN_POINT ( 'NONE',  ( 28.24533480114369866, 202.3655582339692103, -16.73015311598867783 ) ) ;
#13093 = ORIENTED_EDGE ( 'NONE', *, *, #1103, .T. ) ;
#13094 = VERTEX_POINT ( 'NONE', #1769 ) ;
#13095 = CARTESIAN_POINT ( 'NONE',  ( 14.93242934743711814, 20.00000000000000355, -15.00000000000000000 ) ) ;
#13096 = DIRECTION ( 'NONE',  ( 1.000000000000000000, 0.000000000000000000, 0.000000000000000000 ) ) ;
#13097 = ORIENTED_EDGE ( 'NONE', *, *, #8936, .F. ) ;
#13098 = CARTESIAN_POINT ( 'NONE',  ( -86.00000000000002842, 146.6227766016838245, -24.49489742783179480 ) ) ;
#13099 = CARTESIAN_POINT ( 'NONE',  ( 14.92136712345229554, 126.5341449364669728, -7.654582290614115436 ) ) ;
#13100 = EDGE_LOOP ( 'NONE', ( #11197, #11725, #14734, #11065 ) ) ;
#13101 = DIRECTION ( 'NONE',  ( 1.000000000000000000, 0.000000000000000000, 0.000000000000000000 ) ) ;
#13102 = FACE_OUTER_BOUND ( 'NONE', #2264, .T. ) ;
#13103 = EDGE_CURVE ( 'NONE', #12728, #6874, #3597, .T. ) ;
#13104 = LINE ( 'NONE', #3728, #4144 ) ;
#13105 = DIRECTION ( 'NONE',  ( -1.000000000000000000, 0.000000000000000000, 0.000000000000000000 ) ) ;
#13106 = CARTESIAN_POINT ( 'NONE',  ( -17.59086657693884703, 18.00000000000000000, 22.42595686383721443 ) ) ;
#13107 = FACE_OUTER_BOUND ( 'NONE', #10018, .T. ) ;
#13108 = CARTESIAN_POINT ( 'NONE',  ( 37.99999999999999289, 18.00000000000000355, 0.000000000000000000 ) ) ;
#13109 = ORIENTED_EDGE ( 'NONE', *, *, #6577, .F. ) ;
#13110 = LINE ( 'NONE', #2053, #6175 ) ;
#13111 = ADVANCED_FACE ( 'NONE', ( #703 ), #15310, .F. ) ;
#13112 = ORIENTED_EDGE ( 'NONE', *, *, #1387, .F. ) ;
#13113 = ADVANCED_FACE ( 'NONE', ( #11406 ), #4451, .F. ) ;
#13114 = FACE_OUTER_BOUND ( 'NONE', #8055, .T. ) ;
#13115 = EDGE_CURVE ( 'NONE', #13379, #16488, #4518, .T. ) ;
#13116 = CARTESIAN_POINT ( 'NONE',  ( -11.98734322101359240, 18.00000000000000355, -24.50584837321702736 ) ) ;
#13117 = ORIENTED_EDGE ( 'NONE', *, *, #1454, .F. ) ;
#13118 = CARTESIAN_POINT ( 'NONE',  ( -10.04118010627649049, 19.99999999999999645, 24.87462214923097648 ) ) ;
#13119 = CARTESIAN_POINT ( 'NONE',  ( 14.09268385650717015, 127.7503171827756034, 9.071975374176082241 ) ) ;
#13120 = CARTESIAN_POINT ( 'NONE',  ( 29.53214135918837968, 19.99999999999999645, 18.68621337608103516 ) ) ;
#13121 = B_SPLINE_CURVE_WITH_KNOTS ( 'NONE', 3,
 ( #8750, #8566, #12644, #4675 ),
 .UNSPECIFIED., .F., .F.,
 ( 4, 4 ),
 ( 0.000000000000000000, 0.003888888888888887042 ),
 .UNSPECIFIED. ) ;
#13122 = AXIS2_PLACEMENT_3D ( 'NONE', #15830, #11659, #17246 ) ;
#13123 = ORIENTED_EDGE ( 'NONE', *, *, #3658, .T. ) ;
#13124 = VECTOR ( 'NONE', #15600, 1000.000000000000114 ) ;
#13125 = DIRECTION ( 'NONE',  ( 1.000000000000000000, 0.000000000000000000, 0.000000000000000000 ) ) ;
#13126 = DIRECTION ( 'NONE',  ( 0.000000000000000000, 0.000000000000000000, -1.000000000000000000 ) ) ;
#13127 = DIRECTION ( 'NONE',  ( -0.01578383822436034076, 0.1110972697184772484, -0.9936841888205766304 ) ) ;
#13128 = CARTESIAN_POINT ( 'NONE',  ( -14.55266450408069723, 18.00000000000000000, -23.76398220081675206 ) ) ;
#13129 = ORIENTED_EDGE ( 'NONE', *, *, #1574, .T. ) ;
#13130 = CARTESIAN_POINT ( 'NONE',  ( -5.000000000000000888, 171.6227766016838245, 0.000000000000000000 ) ) ;
#13131 = ORIENTED_EDGE ( 'NONE', *, *, #4526, .T. ) ;
#13132 = CARTESIAN_POINT ( 'NONE',  ( 27.00061905785951666, 191.4078883217828491, -28.87216486436160423 ) ) ;
#13133 = DIRECTION ( 'NONE',  ( 0.000000000000000000, 0.000000000000000000, 1.000000000000000000 ) ) ;
#13134 = ORIENTED_EDGE ( 'NONE', *, *, #11965, .F. ) ;
#13135 = AXIS2_PLACEMENT_3D ( 'NONE', #9841, #4710, #5864 ) ;
#13136 = VERTEX_POINT ( 'NONE', #794 ) ;
#13137 = ORIENTED_EDGE ( 'NONE', *, *, #4965, .T. ) ;
#13138 = CARTESIAN_POINT ( 'NONE',  ( -87.34664361473880945, 148.1846496461902518, -23.23759988234784046 ) ) ;
#13139 = VERTEX_POINT ( 'NONE', #16903 ) ;
#13140 = DIRECTION ( 'NONE',  ( 0.000000000000000000, 0.000000000000000000, 1.000000000000000000 ) ) ;
#13141 = EDGE_CURVE ( 'NONE', #15746, #7447, #16614, .T. ) ;
#13142 = CARTESIAN_POINT ( 'NONE',  ( 27.99999999999998224, 9.999999999999998224, 0.000000000000000000 ) ) ;
#13143 = CARTESIAN_POINT ( 'NONE',  ( 48.00000000000000711, 159.6227766016838814, 5.571800142134975431 ) ) ;
#13144 = AXIS2_PLACEMENT_3D ( 'NONE', #7614, #13105, #15667 ) ;
#13145 = CARTESIAN_POINT ( 'NONE',  ( 31.11555797696667369, 152.5224481282687066, -29.32884290898093838 ) ) ;
#13146 = CARTESIAN_POINT ( 'NONE',  ( 22.87887136921732889, 17.99999999999999645, 6.850254086360624939 ) ) ;
#13147 = CARTESIAN_POINT ( 'NONE',  ( -40.00000000000000711, 0.000000000000000000, -3.469446951953615767E-15 ) ) ;
#13148 = AXIS2_PLACEMENT_3D ( 'NONE', #1411, #12020, #16197 ) ;
#13149 = EDGE_LOOP ( 'NONE', ( #3356, #4111, #2928, #13036 ) ) ;
#13150 = DIRECTION ( 'NONE',  ( -0.000000000000000000, -0.000000000000000000, 1.000000000000000000 ) ) ;
#13151 = CARTESIAN_POINT ( 'NONE',  ( 15.59275333247216366, 29.99107914678833353, -15.00000000000000000 ) ) ;
#13152 = CARTESIAN_POINT ( 'NONE',  ( -20.85786437626906675, 124.1421356237309652, -14.99999999999998401 ) ) ;
#13153 = CARTESIAN_POINT ( 'NONE',  ( 39.99999999999998579, 4.000000000000000000, -30.00000000000001066 ) ) ;
#13154 = CARTESIAN_POINT ( 'NONE',  ( 24.93507336697352628, 29.86842105263157876, 4.999999999999999112 ) ) ;
#13155 = ORIENTED_EDGE ( 'NONE', *, *, #1162, .T. ) ;
#13156 = DIRECTION ( 'NONE',  ( 0.000000000000000000, 0.000000000000000000, -1.000000000000000000 ) ) ;
#13157 = VECTOR ( 'NONE', #4838, 1000.000000000000000 ) ;
#13158 = CYLINDRICAL_SURFACE ( 'NONE', #286, 6.000000000000005329 ) ;
#13159 = VECTOR ( 'NONE', #17407, 1000.000000000000000 ) ;
#13160 = ORIENTED_EDGE ( 'NONE', *, *, #8135, .F. ) ;
#13161 = CARTESIAN_POINT ( 'NONE',  ( -80.00000000000002842, 146.6227766016838245, -16.00000000000000000 ) ) ;
#13162 = VECTOR ( 'NONE', #6692, 1000.000000000000000 ) ;
#13163 = DIRECTION ( 'NONE',  ( -1.000000000000000000, -0.000000000000000000, -0.000000000000000000 ) ) ;
#13164 = AXIS2_PLACEMENT_3D ( 'NONE', #14663, #2627, #7744 ) ;
#13165 = ORIENTED_EDGE ( 'NONE', *, *, #13661, .T. ) ;
#13166 = EDGE_CURVE ( 'NONE', #4295, #6662, #6184, .T. ) ;
#13167 = EDGE_CURVE ( 'NONE', #5890, #15563, #13500, .T. ) ;
#13168 = CARTESIAN_POINT ( 'NONE',  ( -82.23503736807776932, 142.1468147500167447, 14.83914868552980515 ) ) ;
#13169 = ADVANCED_FACE ( 'NONE', ( #7164 ), #12561, .T. ) ;
#13170 = CARTESIAN_POINT ( 'NONE',  ( 16.75727253400481942, 18.00000000000114397, -12.82782196133976704 ) ) ;
#13171 = CARTESIAN_POINT ( 'NONE',  ( -84.98839123081494051, 143.2703805450037464, -20.52792728560773838 ) ) ;
#13172 = FACE_OUTER_BOUND ( 'NONE', #11459, .T. ) ;
#13173 = AXIS2_PLACEMENT_3D ( 'NONE', #1728, #654, #1805 ) ;
#13174 = ORIENTED_EDGE ( 'NONE', *, *, #3993, .T. ) ;
#13175 = DIRECTION ( 'NONE',  ( 1.000000000000000000, 0.000000000000000000, 0.000000000000000000 ) ) ;
#13176 = CARTESIAN_POINT ( 'NONE',  ( 7.655193733048226257, 144.1839557653416080, 18.33333333333333925 ) ) ;
#13177 = AXIS2_PLACEMENT_3D ( 'NONE', #8811, #4828, #667 ) ;
#13178 = DIRECTION ( 'NONE',  ( -1.000000000000000000, 0.000000000000000000, 0.000000000000000000 ) ) ;
#13179 = ORIENTED_EDGE ( 'NONE', *, *, #11201, .T. ) ;
#13180 = ORIENTED_EDGE ( 'NONE', *, *, #2566, .F. ) ;
#13181 = DIRECTION ( 'NONE',  ( 0.000000000000000000, 0.000000000000000000, -1.000000000000000000 ) ) ;
#13182 = ORIENTED_EDGE ( 'NONE', *, *, #1328, .T. ) ;
#13183 = CARTESIAN_POINT ( 'NONE',  ( -95.00000000000000000, 201.6227766016838245, 0.000000000000000000 ) ) ;
#13184 = AXIS2_PLACEMENT_3D ( 'NONE', #6570, #7980, #17362 ) ;
#13185 = CARTESIAN_POINT ( 'NONE',  ( 12.95626684960129893, 129.1819364320672321, -10.30967895453046879 ) ) ;
#13186 = ORIENTED_EDGE ( 'NONE', *, *, #6173, .T. ) ;
#13187 = CARTESIAN_POINT ( 'NONE',  ( 32.99999999999998579, 9.999999999999998224, 0.000000000000000000 ) ) ;
#13188 = CIRCLE ( 'NONE', #9227, 2.500000000000002220 ) ;
#13189 = FACE_OUTER_BOUND ( 'NONE', #4369, .T. ) ;
#13190 = CONICAL_SURFACE ( 'NONE', #3015, 1732.050807568857181, 1.047197551196592746 ) ;
#13191 = FACE_OUTER_BOUND ( 'NONE', #11400, .T. ) ;
#13192 = CARTESIAN_POINT ( 'NONE',  ( 196.0000000000000000, 167.6227766016838814, 16.92820660268601429 ) ) ;
#13193 = DIRECTION ( 'NONE',  ( 1.000000000000000000, 0.000000000000000000, -0.000000000000000000 ) ) ;
#13194 = CARTESIAN_POINT ( 'NONE',  ( -98.00000000000000000, 171.6227766016838245, -5.000000000000006217 ) ) ;
#13195 = DIRECTION ( 'NONE',  ( 1.000000000000000000, 0.000000000000000000, 0.000000000000000000 ) ) ;
#13196 = CARTESIAN_POINT ( 'NONE',  ( -45.00000000000001421, -20.00000000000000000, 35.00000000000000711 ) ) ;
#13197 = CYLINDRICAL_SURFACE ( 'NONE', #3242, 2.499999999999998668 ) ;
#13198 = CARTESIAN_POINT ( 'NONE',  ( 33.48938398233770641, 141.7273756662291930, -18.20613184929474926 ) ) ;
#13199 = CIRCLE ( 'NONE', #10356, 2.500000000000000000 ) ;
#13200 = ORIENTED_EDGE ( 'NONE', *, *, #499, .F. ) ;
#13201 = CYLINDRICAL_SURFACE ( 'NONE', #2796, 4.000000000000003553 ) ;
#13202 = ORIENTED_EDGE ( 'NONE', *, *, #15006, .T. ) ;
#13203 = LINE ( 'NONE', #13037, #14684 ) ;
#13204 = CIRCLE ( 'NONE', #778, 27.69059892324149175 ) ;
#13205 = DIRECTION ( 'NONE',  ( 0.000000000000000000, 0.000000000000000000, 1.000000000000000000 ) ) ;
#13206 = EDGE_CURVE ( 'NONE', #13633, #5676, #4173, .T. ) ;
#13207 = VERTEX_POINT ( 'NONE', #12017 ) ;
#13208 = EDGE_CURVE ( 'NONE', #17091, #978, #14063, .T. ) ;
#13209 = CARTESIAN_POINT ( 'NONE',  ( -8.766611209709614272, 19.99999999999771916, 14.60748648876205458 ) ) ;
#13210 = CARTESIAN_POINT ( 'NONE',  ( 14.60960092688903700, 138.5353766997065179, 5.001077596137333714 ) ) ;
#13211 = ORIENTED_EDGE ( 'NONE', *, *, #6083, .F. ) ;
#13212 = FACE_OUTER_BOUND ( 'NONE', #14487, .T. ) ;
#13213 = ORIENTED_EDGE ( 'NONE', *, *, #10313, .T. ) ;
#13214 = AXIS2_PLACEMENT_3D ( 'NONE', #8119, #11041, #13531 ) ;
#13215 = DIRECTION ( 'NONE',  ( 0.000000000000000000, 0.000000000000000000, 1.000000000000000000 ) ) ;
#13216 = EDGE_CURVE ( 'NONE', #11533, #14594, #17154, .T. ) ;
#13217 = AXIS2_PLACEMENT_3D ( 'NONE', #4579, #1912, #5901 ) ;
#13218 = DIRECTION ( 'NONE',  ( 0.000000000000000000, 0.000000000000000000, -1.000000000000000000 ) ) ;
#13219 = CARTESIAN_POINT ( 'NONE',  ( -17.86279820300995169, 32.23061541110773476, -7.751589558536285729 ) ) ;
#13220 = CARTESIAN_POINT ( 'NONE',  ( -27.30244652380281778, 18.00000000000000000, -10.27378278477019080 ) ) ;
#13221 = ORIENTED_EDGE ( 'NONE', *, *, #5015, .T. ) ;
#13222 = FACE_OUTER_BOUND ( 'NONE', #4686, .T. ) ;
#13223 = ORIENTED_EDGE ( 'NONE', *, *, #10013, .F. ) ;
#13224 = CARTESIAN_POINT ( 'NONE',  ( 30.46084342859877836, 190.6362156748385530, -29.38520182610346509 ) ) ;
#13225 = FACE_OUTER_BOUND ( 'NONE', #16333, .T. ) ;
#13226 = ORIENTED_EDGE ( 'NONE', *, *, #6017, .F. ) ;
#13227 = VECTOR ( 'NONE', #11284, 1000.000000000000000 ) ;
#13228 = ORIENTED_EDGE ( 'NONE', *, *, #8512, .T. ) ;
#13229 = ORIENTED_EDGE ( 'NONE', *, *, #8514, .T. ) ;
#13230 = ADVANCED_FACE ( 'NONE', ( #7760 ), #3709, .F. ) ;
#13231 = TOROIDAL_SURFACE ( 'NONE', #802, 14.16444493696511486, 5.000000000000000000 ) ;
#13232 = CARTESIAN_POINT ( 'NONE',  ( -74.54894360611541515, 151.7804781109684029, -26.36917907415269013 ) ) ;
#13233 = ADVANCED_FACE ( 'NONE', ( #6271 ), #2287, .T. ) ;
#13234 = ORIENTED_EDGE ( 'NONE', *, *, #17266, .F. ) ;
#13235 = DIRECTION ( 'NONE',  ( 1.000000000000000000, 0.000000000000000000, 0.000000000000000000 ) ) ;
#13236 = CARTESIAN_POINT ( 'NONE',  ( 27.99999999999998224, 9.999999999999998224, 0.000000000000000000 ) ) ;
#13237 = EDGE_CURVE ( 'NONE', #16986, #15051, #3526, .T. ) ;
#13238 = DIRECTION ( 'NONE',  ( -0.000000000000000000, -0.000000000000000000, 1.000000000000000000 ) ) ;
#13239 = EDGE_CURVE ( 'NONE', #9957, #16088, #5301, .T. ) ;
#13240 = CARTESIAN_POINT ( 'NONE',  ( 29.52501904231387897, 152.6213468612617419, -29.39295273708633971 ) ) ;
#13241 = CARTESIAN_POINT ( 'NONE',  ( 21.03896850327926060, 17.99999999999885247, 10.35865908471247643 ) ) ;
#13242 = CARTESIAN_POINT ( 'NONE',  ( -168.0000000000000284, 178.2321571572880146, 0.000000000000000000 ) ) ;
#13243 = AXIS2_PLACEMENT_3D ( 'NONE', #10885, #5230, #1342 ) ;
#13244 = VECTOR ( 'NONE', #13943, 1000.000000000000000 ) ;
#13245 = ORIENTED_EDGE ( 'NONE', *, *, #12250, .F. ) ;
#13246 = CARTESIAN_POINT ( 'NONE',  ( -73.00000000000001421, 171.6227766016838245, -5.000000000000006217 ) ) ;
#13247 = LINE ( 'NONE', #17402, #7755 ) ;
#13248 = DIRECTION ( 'NONE',  ( 0.000000000000000000, 1.000000000000000000, 0.000000000000000000 ) ) ;
#13249 = DIRECTION ( 'NONE',  ( 0.000000000000000000, 0.000000000000000000, -1.000000000000000000 ) ) ;
#13250 = CARTESIAN_POINT ( 'NONE',  ( -27.98221281341758626, 19.99999999999999645, -6.321711414556861364 ) ) ;
#13251 = B_SPLINE_CURVE_WITH_KNOTS ( 'NONE', 3,
 ( #10422, #12117, #17155, #2466, #10696, #12018, #13176, #9095 ),
 .UNSPECIFIED., .F., .F.,
 ( 4, 2, 2, 4 ),
 ( 0.01981773175714084123, 0.02208185334846130693, 0.02434597493978176916, 0.02887421812242269709 ),
 .UNSPECIFIED. ) ;
#13252 = ORIENTED_EDGE ( 'NONE', *, *, #16758, .T. ) ;
#13253 = CARTESIAN_POINT ( 'NONE',  ( -151.9615242270660929, 171.6227766016838245, 0.000000000000000000 ) ) ;
#13254 = EDGE_CURVE ( 'NONE', #17478, #16965, #13514, .T. ) ;
#13255 = CARTESIAN_POINT ( 'NONE',  ( 31.12398805554424541, 201.4991975277559106, 14.01484360552157327 ) ) ;
#13256 = ORIENTED_EDGE ( 'NONE', *, *, #680, .T. ) ;
#13257 = CARTESIAN_POINT ( 'NONE',  ( 39.99999999999998579, 4.000000000000007105, 30.00000000000001421 ) ) ;
#13259 = FACE_OUTER_BOUND ( 'NONE', #7888, .T. ) ;
#13258 = AXIS2_PLACEMENT_3D ( 'NONE', #9527, #14935, #12542 ) ;
#13260 = ORIENTED_EDGE ( 'NONE', *, *, #16099, .T. ) ;
#13261 = CARTESIAN_POINT ( 'NONE',  ( -84.46916791769895383, 144.3624319200459070, 18.60312384224724980 ) ) ;
#13262 = CARTESIAN_POINT ( 'NONE',  ( 14.93242934743710570, 30.00000000000000000, -13.00000000000000178 ) ) ;
#13263 = CARTESIAN_POINT ( 'NONE',  ( -78.94173059828752059, 140.7111270992951120, -16.41570701070895311 ) ) ;
#13264 = CARTESIAN_POINT ( 'NONE',  ( -27.29618490519992591, 19.99999999999999645, 10.29570512375934399 ) ) ;
#13265 = VERTEX_POINT ( 'NONE', #6349 ) ;
#13266 = DIRECTION ( 'NONE',  ( 0.000000000000000000, 0.000000000000000000, 1.000000000000000000 ) ) ;
#13267 = AXIS2_PLACEMENT_3D ( 'NONE', #6185, #4938, #9984 ) ;
#13268 = CARTESIAN_POINT ( 'NONE',  ( -207.8780901672883772, 173.0692040606395778, -5.343448167864359277 ) ) ;
#13269 = CONICAL_SURFACE ( 'NONE', #14124, 2.500000000000002220, 1.029744260000002631 ) ;
#13270 = FACE_OUTER_BOUND ( 'NONE', #2887, .T. ) ;
#13271 = AXIS2_PLACEMENT_3D ( 'NONE', #1897, #16692, #11276 ) ;
#13272 = EDGE_CURVE ( 'NONE', #7418, #4419, #954, .T. ) ;
#13273 = ADVANCED_FACE ( 'NONE', ( #10595 ), #11744, .F. ) ;
#13274 = EDGE_CURVE ( 'NONE', #12800, #14446, #2189, .T. ) ;
#13275 = VERTEX_POINT ( 'NONE', #15916 ) ;
#13276 = ORIENTED_EDGE ( 'NONE', *, *, #3391, .F. ) ;
#13277 = CARTESIAN_POINT ( 'NONE',  ( 12.97014296496520736, 138.3438685529228565, -12.30864880703445152 ) ) ;
#13278 = ORIENTED_EDGE ( 'NONE', *, *, #10636, .T. ) ;
#13279 = CARTESIAN_POINT ( 'NONE',  ( -82.81127788294642755, 151.9278302392748685, -28.93306197017449222 ) ) ;
#13280 = CARTESIAN_POINT ( 'NONE',  ( 13.53786153804126435, 143.5554826938402755, -17.35616514752890183 ) ) ;
#13281 = CIRCLE ( 'NONE', #15817, 19.49999999999999645 ) ;
#13282 = ORIENTED_EDGE ( 'NONE', *, *, #8795, .T. ) ;
#13283 = DIRECTION ( 'NONE',  ( 0.000000000000000000, 0.000000000000000000, 1.000000000000000000 ) ) ;
#13284 = CARTESIAN_POINT ( 'NONE',  ( 30.00000000000001066, 146.6227766016838245, -16.00000000000000000 ) ) ;
#13285 = AXIS2_PLACEMENT_3D ( 'NONE', #13307, #8066, #11879 ) ;
#13286 = CARTESIAN_POINT ( 'NONE',  ( -68.00000000000000000, 171.6227766016838245, 0.000000000000000000 ) ) ;
#13287 = DIRECTION ( 'NONE',  ( 0.000000000000000000, 1.000000000000000000, 0.000000000000000000 ) ) ;
#13288 = DIRECTION ( 'NONE',  ( 0.000000000000000000, 0.000000000000000000, 1.000000000000000000 ) ) ;
#13289 = CARTESIAN_POINT ( 'NONE',  ( 22.87887136921732889, 17.99999999999999645, -6.850254086360624939 ) ) ;
#13290 = CARTESIAN_POINT ( 'NONE',  ( -725.0000000000000000, 19.99999999999995737, -4.999999999999999112 ) ) ;
#13291 = FACE_OUTER_BOUND ( 'NONE', #2337, .T. ) ;
#13292 = DIRECTION ( 'NONE',  ( 1.000000000000000000, 0.000000000000000000, 0.000000000000000000 ) ) ;
#13293 = ORIENTED_EDGE ( 'NONE', *, *, #10540, .T. ) ;
#13294 = DIRECTION ( 'NONE',  ( -1.000000000000000000, -6.938893903907228378E-16, -0.000000000000000000 ) ) ;
#13295 = AXIS2_PLACEMENT_3D ( 'NONE', #5031, #14592, #15834 ) ;
#13296 = DIRECTION ( 'NONE',  ( 1.000000000000000000, 0.000000000000000000, 0.000000000000000000 ) ) ;
#13297 = EDGE_CURVE ( 'NONE', #17364, #10657, #3619, .T. ) ;
#13298 = ORIENTED_EDGE ( 'NONE', *, *, #14141, .F. ) ;
#13299 = FACE_OUTER_BOUND ( 'NONE', #2156, .T. ) ;
#13300 = AXIS2_PLACEMENT_3D ( 'NONE', #13284, #1327, #10526 ) ;
#13301 = B_SPLINE_CURVE_WITH_KNOTS ( 'NONE', 3,
 ( #2459, #2556, #1133, #10508, #9091, #15913, #16190, #7948, #12014, #17417, #1217, #2284, #8025, #17148, #6712, #12112, #13263, #10592, #14497, #6538, #5197, #10416, #13353, #2640, #13085, #13436, #3704, #10691, #7757, #1307, #17516, #3979, #9362, #10781, #13171, #6622, #3781, #14767, #4060, #1041, #6441, #9437 ),
 .UNSPECIFIED., .F., .F.,
 ( 4, 2, 2, 2, 2, 2, 2, 2, 2, 2, 2, 2, 2, 2, 2, 2, 2, 2, 2, 2, 4 ),
 ( 0.000000000000000000, 0.003174452718035057977, 0.004761679077052617323, 0.006348905436070176669, 0.007936131795087736016, 0.009523358154105295362, 0.01031697133361409238, 0.01111058451312288940, 0.01190419769263168642, 0.01230100428238609968, 0.01269781087214051120, 0.01349142405164937761, 0.01428503723115824228, 0.01507865041066711043, 0.01587226359017597510, 0.01745948994919370445, 0.01904671630821143033, 0.02063394266722915621, 0.02222116902624688556, 0.02380839538526460797, 0.02539562174428233732 ),
 .UNSPECIFIED. ) ;
#13302 = CARTESIAN_POINT ( 'NONE',  ( 48.00000000000000711, 167.6227766016838814, -21.92820660268601074 ) ) ;
#13303 = ORIENTED_EDGE ( 'NONE', *, *, #10198, .T. ) ;
#13304 = CARTESIAN_POINT ( 'NONE',  ( 27.50000000000001066, 146.6227766016838245, 0.000000000000000000 ) ) ;
#13305 = CARTESIAN_POINT ( 'NONE',  ( 13.82444641086477866, 138.9325364249946517, 8.217559156358525740 ) ) ;
#13306 = ORIENTED_EDGE ( 'NONE', *, *, #15094, .F. ) ;
#13307 = CARTESIAN_POINT ( 'NONE',  ( 48.00000000000000711, 159.6227766016838814, -5.571800142134975431 ) ) ;
#13308 = AXIS2_PLACEMENT_3D ( 'NONE', #14773, #6720, #5562 ) ;
#13309 = ORIENTED_EDGE ( 'NONE', *, *, #9681, .T. ) ;
#13310 = AXIS2_PLACEMENT_3D ( 'NONE', #3068, #16529, #8471 ) ;
#13311 = CARTESIAN_POINT ( 'NONE',  ( -32.65879391391417386, 101.1479710282390840, 4.574240649584753626 ) ) ;
#13312 = DIRECTION ( 'NONE',  ( 0.000000000000000000, 0.000000000000000000, 1.000000000000000000 ) ) ;
#13313 = FACE_OUTER_BOUND ( 'NONE', #11173, .T. ) ;
#13314 = CARTESIAN_POINT ( 'NONE',  ( -15.84134677353521070, 32.63429591450738343, -7.614689697697072823 ) ) ;
#13315 = EDGE_CURVE ( 'NONE', #5242, #16418, #6153, .T. ) ;
#13316 = VERTEX_POINT ( 'NONE', #6541 ) ;
#13317 = DIRECTION ( 'NONE',  ( -6.938893903907228378E-16, 1.000000000000000000, 0.000000000000000000 ) ) ;
#13318 = ORIENTED_EDGE ( 'NONE', *, *, #16378, .F. ) ;
#13319 = CARTESIAN_POINT ( 'NONE',  ( -207.7491074081026454, 175.3340477608625463, -3.959435662344279905 ) ) ;
#13320 = FACE_OUTER_BOUND ( 'NONE', #6608, .T. ) ;
#13321 = AXIS2_PLACEMENT_3D ( 'NONE', #8093, #3957, #52 ) ;
#13322 = VERTEX_POINT ( 'NONE', #14327 ) ;
#13323 = VERTEX_POINT ( 'NONE', #10513 ) ;
#13324 = ORIENTED_EDGE ( 'NONE', *, *, #2681, .T. ) ;
#13325 = CARTESIAN_POINT ( 'NONE',  ( -73.91918570238915720, 151.0194919042433241, -25.77925661938085611 ) ) ;
#13326 = ORIENTED_EDGE ( 'NONE', *, *, #11163, .T. ) ;
#13327 = DIRECTION ( 'NONE',  ( 0.000000000000000000, 0.000000000000000000, 1.000000000000000000 ) ) ;
#13328 = CARTESIAN_POINT ( 'NONE',  ( 27.48361012695488981, 138.6227766016838245, -1.225897272825924533 ) ) ;
#13329 = CARTESIAN_POINT ( 'NONE',  ( -80.00000000000002842, 146.6227766016838245, -13.00000000000000000 ) ) ;
#13330 = CARTESIAN_POINT ( 'NONE',  ( 34.82472073241385857, 150.2116474542520166, -27.68948087834226968 ) ) ;
#13331 = AXIS2_PLACEMENT_3D ( 'NONE', #6944, #12259, #1197 ) ;
#13332 = FACE_BOUND ( 'NONE', #5886, .T. ) ;
#13333 = CARTESIAN_POINT ( 'NONE',  ( -82.87337507697658623, 150.7186413122655892, 25.53493815998142935 ) ) ;
#13334 = EDGE_CURVE ( 'NONE', #11751, #7408, #4187, .T. ) ;
#13335 = VERTEX_POINT ( 'NONE', #15649 ) ;
#13336 = CARTESIAN_POINT ( 'NONE',  ( -79.44857787935347915, 202.6030615872001022, -16.28580987144871628 ) ) ;
#13337 = CARTESIAN_POINT ( 'NONE',  ( 16.24588547270996131, 29.98230316816100327, -14.93526533897157726 ) ) ;
#13338 = PLANE ( 'NONE',  #4829 ) ;
#13339 = DIRECTION ( 'NONE',  ( 0.000000000000000000, -1.000000000000000000, 8.673617379884035472E-17 ) ) ;
#13340 = CARTESIAN_POINT ( 'NONE',  ( 37.50000000000000711, 196.6227766016838245, -21.54065922853802562 ) ) ;
#13341 = VERTEX_POINT ( 'NONE', #14681 ) ;
#13342 = CARTESIAN_POINT ( 'NONE',  ( -87.50000000000004263, 146.6227766016838245, -21.54065922853802562 ) ) ;
#13343 = PRODUCT_DEFINITION ( 'UNKNOWN', '', #7837, #1651 ) ;
#13344 = EDGE_CURVE ( 'NONE', #15814, #16730, #13007, .T. ) ;
#13345 = EDGE_CURVE ( 'NONE', #8508, #10480, #2196, .T. ) ;
#13346 = CARTESIAN_POINT ( 'NONE',  ( 25.98211652881812483, 199.6128501304145004, 17.48539201980446123 ) ) ;
#13347 = EDGE_LOOP ( 'NONE', ( #9327, #17414, #275, #14983, #7660, #12056 ) ) ;
#13348 = FACE_BOUND ( 'NONE', #11020, .T. ) ;
#13349 = CARTESIAN_POINT ( 'NONE',  ( -100.0000000000000000, 201.6227766016838245, 0.000000000000000000 ) ) ;
#13350 = ORIENTED_EDGE ( 'NONE', *, *, #17288, .F. ) ;
#13351 = CARTESIAN_POINT ( 'NONE',  ( -75.00000000000002842, 146.3163998792643952, 21.18507967179267482 ) ) ;
#13352 = CARTESIAN_POINT ( 'NONE',  ( -16.30611068361787019, 32.76923076923078781, 4.999999999999999112 ) ) ;
#13353 = CARTESIAN_POINT ( 'NONE',  ( -80.52893385407348603, 140.6403763931701576, -16.28177936134992976 ) ) ;
#13354 = CARTESIAN_POINT ( 'NONE',  ( -24.80114670877660643, 19.99999999999999289, 15.70637264050929538 ) ) ;
#13355 = ORIENTED_EDGE ( 'NONE', *, *, #10851, .T. ) ;
#13356 = DIRECTION ( 'NONE',  ( 1.000000000000000000, -0.000000000000000000, -0.000000000000000000 ) ) ;
#13357 = DIRECTION ( 'NONE',  ( -1.000000000000000000, 0.000000000000000000, 0.000000000000000000 ) ) ;
#13358 = PLANE ( 'NONE',  #15 ) ;
#13359 = DIRECTION ( 'NONE',  ( 0.000000000000000000, 0.000000000000000000, 1.000000000000000000 ) ) ;
#13360 = ORIENTED_EDGE ( 'NONE', *, *, #7414, .T. ) ;
#13361 = CARTESIAN_POINT ( 'NONE',  ( -50.00000000000000000, 206.6227766016838245, 2.143131898507868248E-15 ) ) ;
#13362 = ORIENTED_EDGE ( 'NONE', *, *, #14410, .T. ) ;
#13363 = CARTESIAN_POINT ( 'NONE',  ( -82.99933485059881377, 151.8237148210350540, -28.86201951371925389 ) ) ;
#13364 = CARTESIAN_POINT ( 'NONE',  ( 9.414336857517209722, 132.5946763488762770, -12.41924194405873649 ) ) ;
#13365 = ORIENTED_EDGE ( 'NONE', *, *, #7208, .T. ) ;
#13366 = DIRECTION ( 'NONE',  ( -1.000000000000000000, 0.000000000000000000, 0.000000000000000000 ) ) ;
#13367 = CARTESIAN_POINT ( 'NONE',  ( -32.02886766642084382, 119.9418479153537334, -5.500000000000000000 ) ) ;
#13368 = DIRECTION ( 'NONE',  ( 1.000000000000000000, 0.000000000000000000, 0.000000000000000000 ) ) ;
#13369 = ADVANCED_FACE ( 'NONE', ( #8381 ), #12466, .T. ) ;
#13370 = DIRECTION ( 'NONE',  ( -0.08715574274764689711, 0.9961946980917465444, 0.000000000000000000 ) ) ;
#13371 = CARTESIAN_POINT ( 'NONE',  ( -725.0000000000000000, 19.99999999999995737, -4.999999999999997335 ) ) ;
#13372 = CARTESIAN_POINT ( 'NONE',  ( 22.81311145407750374, 18.00000000000113687, -7.108351238697862229 ) ) ;
#13373 = DIRECTION ( 'NONE',  ( 0.000000000000000000, 0.000000000000000000, 1.000000000000000000 ) ) ;
#13374 = CARTESIAN_POINT ( 'NONE',  ( -27.98221281347032274, 18.00000000000000000, 4.999999999999996447 ) ) ;
#13375 = DIRECTION ( 'NONE',  ( -1.000000000000000000, -0.000000000000000000, 0.000000000000000000 ) ) ;
#13376 = CARTESIAN_POINT ( 'NONE',  ( 24.65551710168432109, 143.8733932267928992, -21.33602313251873639 ) ) ;
#13377 = EDGE_LOOP ( 'NONE', ( #2245, #7462, #14220, #9570 ) ) ;
#13378 = CARTESIAN_POINT ( 'NONE',  ( -68.00000000000000000, 154.3022685259950038, 9.999999999999900524 ) ) ;
#13379 = VERTEX_POINT ( 'NONE', #16274 ) ;
#13380 = CARTESIAN_POINT ( 'NONE',  ( 1.559999999999998943, -1.299038105676664223, 0.7500000000000006661 ) ) ;
#13381 = CARTESIAN_POINT ( 'NONE',  ( -19.25702671965663626, 18.00000000000000355, -21.36300512502526061 ) ) ;
#13382 = EDGE_LOOP ( 'NONE', ( #17121, #10858, #5994, #12712 ) ) ;
#13383 = CARTESIAN_POINT ( 'NONE',  ( -12.63609539511577218, 19.99999999999999645, 24.35132453916816431 ) ) ;
#13384 = CARTESIAN_POINT ( 'NONE',  ( 13.63270490666636192, 138.8028880870465969, 3.449993069226350517 ) ) ;
#13385 = ORIENTED_EDGE ( 'NONE', *, *, #9747, .F. ) ;
#13386 = PLANE ( 'NONE',  #7906 ) ;
#13387 = EDGE_LOOP ( 'NONE', ( #11785, #1860 ) ) ;
#13388 = ADVANCED_FACE ( 'NONE', ( #4146 ), #5394, .F. ) ;
#13389 = EDGE_CURVE ( 'NONE', #9250, #12210, #15023, .T. ) ;
#13390 = EDGE_CURVE ( 'NONE', #554, #2195, #11515, .T. ) ;
#13391 = EDGE_CURVE ( 'NONE', #2395, #2095, #7560, .T. ) ;
#13392 = LINE ( 'NONE', #6666, #4978 ) ;
#13393 = CARTESIAN_POINT ( 'NONE',  ( 35.08450508553749358, 191.0841166510128062, -26.65369102675423818 ) ) ;
#13394 = EDGE_CURVE ( 'NONE', #11331, #11495, #4465, .T. ) ;
#13395 = DIRECTION ( 'NONE',  ( 1.000000000000000000, -0.000000000000000000, -0.000000000000000000 ) ) ;
#13396 = CARTESIAN_POINT ( 'NONE',  ( -26.11264420168958722, 18.00000000000000000, -13.35921939055965524 ) ) ;
#13397 = ORIENTED_EDGE ( 'NONE', *, *, #77, .T. ) ;
#13398 = CARTESIAN_POINT ( 'NONE',  ( 27.12662492302345996, 150.7186413122655892, 25.53493815998142225 ) ) ;
#13399 = VERTEX_POINT ( 'NONE', #6972 ) ;
#13400 = CARTESIAN_POINT ( 'NONE',  ( -208.0706889292728476, 175.9374385743225560, -3.820176503624857389 ) ) ;
#13401 = LINE ( 'NONE', #5352, #6113 ) ;
#13402 = ORIENTED_EDGE ( 'NONE', *, *, #15800, .T. ) ;
#13403 = ORIENTED_EDGE ( 'NONE', *, *, #2848, .T. ) ;
#13404 = ORIENTED_EDGE ( 'NONE', *, *, #8034, .F. ) ;
#13405 = VECTOR ( 'NONE', #3094, 1000.000000000000000 ) ;
#13406 = ADVANCED_FACE ( 'NONE', ( #9365 ), #17521, .F. ) ;
#13407 = DIRECTION ( 'NONE',  ( 0.000000000000000000, -1.000000000000000000, 6.123233995736762338E-17 ) ) ;
#13408 = ORIENTED_EDGE ( 'NONE', *, *, #2716, .T. ) ;
#13409 = APPLICATION_PROTOCOL_DEFINITION ( 'draft international standard', 'automotive_design', 1998, #1332 ) ;
#13410 = DIRECTION ( 'NONE',  ( 0.000000000000000000, 1.000000000000000000, 0.000000000000000000 ) ) ;
#13411 = CARTESIAN_POINT ( 'NONE',  ( -18.09555036921010540, 32.27673591576833445, 6.733025906873759681 ) ) ;
#13412 = CARTESIAN_POINT ( 'NONE',  ( 24.27081732008962334, 148.4136790374692509, -26.19897850971621978 ) ) ;
#13413 = CARTESIAN_POINT ( 'NONE',  ( -73.00000000000001421, 171.6227766016838245, 19.49999999999999645 ) ) ;
#13414 = CARTESIAN_POINT ( 'NONE',  ( -77.13041205501343711, 150.7324203247391381, 25.54751979981075394 ) ) ;
#13415 = CIRCLE ( 'NONE', #10586, 25.46898629924947244 ) ;
#13416 = ORIENTED_EDGE ( 'NONE', *, *, #14141, .T. ) ;
#13417 = CARTESIAN_POINT ( 'NONE',  ( -84.78531899738449340, 200.2598589880381894, -20.12830716182790880 ) ) ;
#13418 = CARTESIAN_POINT ( 'NONE',  ( -50.00000000000000000, 171.6227766016838245, 0.000000000000000000 ) ) ;
#13420 = DIRECTION ( 'NONE',  ( -1.000000000000000000, -0.000000000000000000, -0.000000000000000000 ) ) ;
#13419 = AXIS2_PLACEMENT_3D ( 'NONE', #8414, #7093, #12494 ) ;
#13421 = DIRECTION ( 'NONE',  ( -1.000000000000000000, -0.000000000000000000, -0.000000000000000000 ) ) ;
#13422 = DIRECTION ( 'NONE',  ( 1.000000000000000000, 0.000000000000000000, 0.000000000000000000 ) ) ;
#13423 = ORIENTED_EDGE ( 'NONE', *, *, #373, .T. ) ;
#13424 = CARTESIAN_POINT ( 'NONE',  ( -45.00000000000000000, 134.2062027339443944, 15.00000000000000000 ) ) ;
#13425 = LINE ( 'NONE', #9938, #10046 ) ;
#13426 = DIRECTION ( 'NONE',  ( 0.000000000000000000, -1.000000000000000000, 0.000000000000000000 ) ) ;
#13427 = ADVANCED_FACE ( 'NONE', ( #1404 ), #2815, .F. ) ;
#13428 = ORIENTED_EDGE ( 'NONE', *, *, #15077, .F. ) ;
#13429 = EDGE_CURVE ( 'NONE', #15454, #9311, #6725, .T. ) ;
#13430 = CARTESIAN_POINT ( 'NONE',  ( 196.0000000000000000, 175.6227766016838530, -19.42820660268601074 ) ) ;
#13431 = AXIS2_PLACEMENT_3D ( 'NONE', #30, #2771, #8162 ) ;
#13432 = ORIENTED_EDGE ( 'NONE', *, *, #460, .F. ) ;
#13433 = CARTESIAN_POINT ( 'NONE',  ( -77.77610210663782198, 142.1412512070565413, 14.82809033015227307 ) ) ;
#13434 = VECTOR ( 'NONE', #8942, 1000.000000000000000 ) ;
#13435 = LINE ( 'NONE', #5117, #8337 ) ;
#13436 = CARTESIAN_POINT ( 'NONE',  ( -81.76357793902667481, 140.8827219813066165, -16.73516917262795189 ) ) ;
#13437 = CARTESIAN_POINT ( 'NONE',  ( -27.98221281347037959, 20.00000000000000355, 5.670874406215274277 ) ) ;
#13438 = ADVANCED_FACE ( 'NONE', ( #6811 ), #13441, .T. ) ;
#13439 = VERTEX_POINT ( 'NONE', #15103 ) ;
#13440 = EDGE_CURVE ( 'NONE', #4201, #9130, #16458, .T. ) ;
#13441 = CYLINDRICAL_SURFACE ( 'NONE', #3037, 2.499999999999999112 ) ;
#13442 = CARTESIAN_POINT ( 'NONE',  ( -80.00000000000002842, 146.6227766016838245, 1.387778780781445676E-14 ) ) ;
#13443 = CARTESIAN_POINT ( 'NONE',  ( -40.00000000000000000, 4.000000000000000000, -30.00000000000000711 ) ) ;
#13444 = FACE_OUTER_BOUND ( 'NONE', #2889, .T. ) ;
#13445 = MECHANICAL_DESIGN_GEOMETRIC_PRESENTATION_REPRESENTATION (  '', ( #14006 ), #9462 ) ;
#13446 = ORIENTED_EDGE ( 'NONE', *, *, #12472, .T. ) ;
#13447 = CARTESIAN_POINT ( 'NONE',  ( 12.82285603306638144, 130.8395207603766153, -12.92896204370639524 ) ) ;
#13448 = ORIENTED_EDGE ( 'NONE', *, *, #13272, .F. ) ;
#13449 = CARTESIAN_POINT ( 'NONE',  ( -79.10703801256936174, 152.5603119736738051, -29.35342143133167170 ) ) ;
#13450 = CARTESIAN_POINT ( 'NONE',  ( 11.58137902169841027, 143.8440485058968363, -17.81491816053495825 ) ) ;
#13451 = ORIENTED_EDGE ( 'NONE', *, *, #4038, .T. ) ;
#13452 = CARTESIAN_POINT ( 'NONE',  ( -27.98221281347037959, 19.99999999999999645, 0.000000000000000000 ) ) ;
#13453 = FACE_OUTER_BOUND ( 'NONE', #294, .T. ) ;
#13454 = AXIS2_PLACEMENT_3D ( 'NONE', #4297, #4379, #10759 ) ;
#13455 = DIRECTION ( 'NONE',  ( 1.000000000000000000, -0.000000000000000000, -0.000000000000000000 ) ) ;
#13456 = VECTOR ( 'NONE', #7150, 1000.000000000000000 ) ;
#13457 = CARTESIAN_POINT ( 'NONE',  ( -24.94987437106622252, 100.0000000000000142, 6.000000000000000000 ) ) ;
#13458 = CYLINDRICAL_SURFACE ( 'NONE', #16319, 2.499999999999998668 ) ;
#13459 = ADVANCED_FACE ( 'NONE', ( #4235 ), #8693, .T. ) ;
#13460 = SHAPE_REPRESENTATION ( 'Variable Speed Trigger Switch assembly', ( #3583 ), #9837 ) ;
#13461 = CARTESIAN_POINT ( 'NONE',  ( 27.13959012325753406, 18.00000000000000000, -20.89788123228700556 ) ) ;
#13462 = CARTESIAN_POINT ( 'NONE',  ( -206.1506185320109239, 122.5792347710271741, -22.63563774299437625 ) ) ;
#13463 = CARTESIAN_POINT ( 'NONE',  ( 27.50000000000000355, 196.6227766016838245, 0.000000000000000000 ) ) ;
#13464 = DIRECTION ( 'NONE',  ( 0.000000000000000000, 0.000000000000000000, 1.000000000000000000 ) ) ;
#13465 = CYLINDRICAL_SURFACE ( 'NONE', #11709, 20.00000000000000355 ) ;
#13466 = VERTEX_POINT ( 'NONE', #2982 ) ;
#13467 = CARTESIAN_POINT ( 'NONE',  ( 10.11940563665161541, 132.7319563576625399, -14.29042643364863885 ) ) ;
#13468 = ORIENTED_EDGE ( 'NONE', *, *, #16262, .T. ) ;
#13469 = PLANE ( 'NONE',  #432 ) ;
#13470 = CIRCLE ( 'NONE', #183, 5.000000000000004441 ) ;
#13471 = CARTESIAN_POINT ( 'NONE',  ( -19.79962810613639945, 18.00000000000000711, -20.97942696524416206 ) ) ;
#13472 = EDGE_CURVE ( 'NONE', #17412, #160, #7000, .T. ) ;
#13473 = AXIS2_PLACEMENT_3D ( 'NONE', #10218, #12796, #7642 ) ;
#13474 = EDGE_LOOP ( 'NONE', ( #5900, #6810, #1229, #1319, #3320 ) ) ;
#13475 = CARTESIAN_POINT ( 'NONE',  ( -17.59086657693882927, 19.99999999999999645, 22.42595686383492293 ) ) ;
#13476 = CARTESIAN_POINT ( 'NONE',  ( 12.08578903453337183, 130.1663611114758510, 11.02150463548631976 ) ) ;
#13477 = VERTEX_POINT ( 'NONE', #7063 ) ;
#13478 = CARTESIAN_POINT ( 'NONE',  ( 19.14963388379468157, 19.99999999999999645, 24.55317681541820463 ) ) ;
#13479 = ORIENTED_EDGE ( 'NONE', *, *, #3118, .F. ) ;
#13480 = LINE ( 'NONE', #9314, #15451 ) ;
#13481 = AXIS2_PLACEMENT_3D ( 'NONE', #7005, #2924, #15130 ) ;
#13482 = VECTOR ( 'NONE', #4022, 1000.000000000000114 ) ;
#13483 = CARTESIAN_POINT ( 'NONE',  ( 34.24679270737827608, 190.4349707265700715, -27.11332964807921897 ) ) ;
#13484 = CARTESIAN_POINT ( 'NONE',  ( 49.99999999999998579, 151.6227766016839098, 3.071800142134974099 ) ) ;
#13485 = AXIS2_PLACEMENT_3D ( 'NONE', #10025, #13868, #15437 ) ;
#13486 = CARTESIAN_POINT ( 'NONE',  ( 27.47046400057530846, 138.6909045376442009, 2.448381753924629756 ) ) ;
#13487 = MECHANICAL_DESIGN_GEOMETRIC_PRESENTATION_REPRESENTATION (  '', ( #12110 ), #14367 ) ;
#13488 = AXIS2_PLACEMENT_3D ( 'NONE', #11128, #8219, #4328 ) ;
#13489 = VERTEX_POINT ( 'NONE', #244 ) ;
#13490 = CARTESIAN_POINT ( 'NONE',  ( -5.000000000000000888, 204.6227766016838245, 2.020667218593133100E-15 ) ) ;
#13491 = ORIENTED_EDGE ( 'NONE', *, *, #1057, .F. ) ;
#13492 = CARTESIAN_POINT ( 'NONE',  ( -86.80614408739177179, 193.4380998888853185, -24.76648413410753946 ) ) ;
#13493 = CARTESIAN_POINT ( 'NONE',  ( -43.00000000000000000, 130.0000000000000000, 0.000000000000000000 ) ) ;
#13494 = EDGE_CURVE ( 'NONE', #5867, #9434, #10381, .T. ) ;
#13495 = EDGE_LOOP ( 'NONE', ( #12518, #12247, #5114, #3701, #16828, #14046, #13093, #6059, #6568, #1549, #16983, #16434, #14470, #10561, #14595 ) ) ;
#13496 = ADVANCED_FACE ( 'NONE', ( #12116 ), #153, .T. ) ;
#13497 = ORIENTED_EDGE ( 'NONE', *, *, #5737, .T. ) ;
#13498 = EDGE_CURVE ( 'NONE', #10197, #16285, #15370, .T. ) ;
#13499 = EDGE_LOOP ( 'NONE', ( #7073, #6681, #4905, #13956 ) ) ;
#13500 = CIRCLE ( 'NONE', #14618, 4.000000000000002665 ) ;
#13502 = CARTESIAN_POINT ( 'NONE',  ( 10.67016715011939176, 138.9541284244158419, 13.78020913810612491 ) ) ;
#13501 = STYLED_ITEM ( 'NONE', ( #17041 ), #4875 ) ;
#13503 = MECHANICAL_DESIGN_GEOMETRIC_PRESENTATION_REPRESENTATION (  '', ( #1347 ), #9241 ) ;
#13504 = ORIENTED_EDGE ( 'NONE', *, *, #3993, .F. ) ;
#13505 = SHAPE_DEFINITION_REPRESENTATION ( #7152, #7924 ) ;
#13506 = DIRECTION ( 'NONE',  ( -1.000000000000000000, -0.000000000000000000, -0.000000000000000000 ) ) ;
#13507 = DIRECTION ( 'NONE',  ( 0.000000000000000000, -0.000000000000000000, -1.000000000000000000 ) ) ;
#13508 = CARTESIAN_POINT ( 'NONE',  ( 19.16569565073602277, 29.91542719746881929, -11.79421528189872070 ) ) ;
#13509 = CARTESIAN_POINT ( 'NONE',  ( -24.93725393319379435, 120.0000000000000284, 5.500000000000000000 ) ) ;
#13510 = DIRECTION ( 'NONE',  ( 1.000000000000000000, 0.000000000000000000, 0.000000000000000000 ) ) ;
#13511 = PRODUCT_DEFINITION_SHAPE ( 'NONE', 'NONE',  #17536 ) ;
#13512 = ORIENTED_EDGE ( 'NONE', *, *, #8022, .F. ) ;
#13513 = CARTESIAN_POINT ( 'NONE',  ( -85.49405842113658593, 199.0592542586747982, -21.73717956246137106 ) ) ;
#13514 = CIRCLE ( 'NONE', #211, 2.500000000000000000 ) ;
#13515 = LINE ( 'NONE', #8011, #12462 ) ;
#13516 = LINE ( 'NONE', #10578, #5810 ) ;
#13517 = CARTESIAN_POINT ( 'NONE',  ( -207.8765633999775275, 173.0709657280817453, 5.341470372219078833 ) ) ;
#13518 = CARTESIAN_POINT ( 'NONE',  ( -71.66708739526794147, 110.0000000000000142, -4.499999999999999112 ) ) ;
#13519 = AXIS2_PLACEMENT_3D ( 'NONE', #14698, #3999, #1325 ) ;
#13520 = CARTESIAN_POINT ( 'NONE',  ( 35.00000000000000711, 146.6227766016838245, 0.000000000000000000 ) ) ;
#13521 = VERTEX_POINT ( 'NONE', #8821 ) ;
#13522 = DIRECTION ( 'NONE',  ( 0.000000000000000000, -1.000000000000000000, 0.000000000000000000 ) ) ;
#13523 = ORIENTED_EDGE ( 'NONE', *, *, #13472, .F. ) ;
#13524 = AXIS2_PLACEMENT_3D ( 'NONE', #9509, #11021, #1200 ) ;
#13525 = DIRECTION ( 'NONE',  ( 1.000000000000000000, 0.000000000000000000, 0.000000000000000000 ) ) ;
#13526 = CONICAL_SURFACE ( 'NONE', #6453, 2.499999999999998668, 1.029744260000002187 ) ;
#13527 = CARTESIAN_POINT ( 'NONE',  ( -95.00000000000000000, 171.6227766016838245, 0.000000000000000000 ) ) ;
#13528 = DIRECTION ( 'NONE',  ( -1.000000000000000000, 0.000000000000000000, 0.000000000000000000 ) ) ;
#13529 = FACE_OUTER_BOUND ( 'NONE', #8203, .T. ) ;
#13530 = VERTEX_POINT ( 'NONE', #12635 ) ;
#13531 = DIRECTION ( 'NONE',  ( 0.000000000000000000, 0.000000000000000000, -1.000000000000000000 ) ) ;
#13532 = DIRECTION ( 'NONE',  ( 0.000000000000000000, 1.000000000000000000, -0.000000000000000000 ) ) ;
#13533 = FACE_OUTER_BOUND ( 'NONE', #12261, .T. ) ;
#13534 = ADVANCED_FACE ( 'NONE', ( #603 ), #3247, .T. ) ;
#13535 = CARTESIAN_POINT ( 'NONE',  ( -100.0000000000000000, 171.6227766016838245, 0.000000000000000000 ) ) ;
#13536 = VECTOR ( 'NONE', #5583, 1000.000000000000114 ) ;
#13537 = AXIS2_PLACEMENT_3D ( 'NONE', #13966, #16795, #15366 ) ;
#13538 = CARTESIAN_POINT ( 'NONE',  ( 21.38051303314620810, 139.8000659834381736, -14.57605648433057510 ) ) ;
#13539 = EDGE_LOOP ( 'NONE', ( #7309, #13813, #2006, #8815 ) ) ;
#13540 = FACE_OUTER_BOUND ( 'NONE', #11672, .T. ) ;
#13541 = FACE_OUTER_BOUND ( 'NONE', #9931, .T. ) ;
#13542 = ORIENTED_EDGE ( 'NONE', *, *, #4223, .T. ) ;
#13543 = DIRECTION ( 'NONE',  ( 1.000000000000000000, 0.000000000000000000, 0.000000000000000000 ) ) ;
#13544 = FACE_OUTER_BOUND ( 'NONE', #7332, .T. ) ;
#13545 = CYLINDRICAL_SURFACE ( 'NONE', #1371, 20.00000000000000355 ) ;
#13546 = AXIS2_PLACEMENT_3D ( 'NONE', #10718, #14787, #2752 ) ;
#13547 = ADVANCED_FACE ( 'NONE', ( #2088 ), #7409, .T. ) ;
#13548 = CIRCLE ( 'NONE', #12976, 2.500000000000002220 ) ;
#13549 = CARTESIAN_POINT ( 'NONE',  ( 34.24368835419660684, 193.9611582889533281, 24.29263104154015096 ) ) ;
#13550 = CONICAL_SURFACE ( 'NONE', #10714, 8.000000000000007105, 0.08726646259970990971 ) ;
#13551 = CARTESIAN_POINT ( 'NONE',  ( 27.99999999999998224, 9.999999999999998224, 11.50215154306610188 ) ) ;
#13552 = CARTESIAN_POINT ( 'NONE',  ( 33.66001102075319551, 18.00000000000000000, -12.05479157725487482 ) ) ;
#13553 = CARTESIAN_POINT ( 'NONE',  ( -208.1430079281944074, 166.0913325906388422, -2.284806080016993590 ) ) ;
#13554 = CARTESIAN_POINT ( 'NONE',  ( -12.80328004466210601, 17.99999999999999645, 4.999999999999999112 ) ) ;
#13555 = CARTESIAN_POINT ( 'NONE',  ( 50.00000000000000000, 196.6227766016838245, 0.000000000000000000 ) ) ;
#13556 = EDGE_CURVE ( 'NONE', #13489, #11737, #16349, .T. ) ;
#13557 = CARTESIAN_POINT ( 'NONE',  ( 49.99999999999998579, 179.6227766016838245, -15.00000337241049486 ) ) ;
#13558 = ORIENTED_EDGE ( 'NONE', *, *, #7811, .F. ) ;
#13559 = CARTESIAN_POINT ( 'NONE',  ( 13.34250444320487361, 130.4016344817123070, -12.56142338728217744 ) ) ;
#13560 = VERTEX_POINT ( 'NONE', #15200 ) ;
#13561 = DIRECTION ( 'NONE',  ( 0.000000000000000000, 0.000000000000000000, -1.000000000000000000 ) ) ;
#13562 = AXIS2_PLACEMENT_3D ( 'NONE', #8588, #4615, #9993 ) ;
#13563 = VECTOR ( 'NONE', #2562, 1000.000000000000000 ) ;
#13564 = EDGE_CURVE ( 'NONE', #11802, #10896, #15636, .T. ) ;
#13565 = CARTESIAN_POINT ( 'NONE',  ( -102.0000000000000142, 171.6227766016838245, 0.000000000000000000 ) ) ;
#13566 = ORIENTED_EDGE ( 'NONE', *, *, #6786, .T. ) ;
#13567 = EDGE_CURVE ( 'NONE', #13780, #16273, #15554, .T. ) ;
#13568 = CARTESIAN_POINT ( 'NONE',  ( -18.25212770525992667, 32.30769230769230660, 4.999999999999998224 ) ) ;
#13569 = VECTOR ( 'NONE', #3699, 1000.000000000000000 ) ;
#13570 = EDGE_CURVE ( 'NONE', #14296, #243, #16632, .T. ) ;
#13571 = CYLINDRICAL_SURFACE ( 'NONE', #13590, 12.00000000000000000 ) ;
#13572 = EDGE_LOOP ( 'NONE', ( #797, #11071, #7276, #14509 ) ) ;
#13573 = CARTESIAN_POINT ( 'NONE',  ( -33.00000000000000711, 171.6227766016838245, 0.000000000000000000 ) ) ;
#13574 = ORIENTED_EDGE ( 'NONE', *, *, #9307, .F. ) ;
#13575 = DIRECTION ( 'NONE',  ( 0.000000000000000000, 0.000000000000000000, 1.000000000000000000 ) ) ;
#13576 = CARTESIAN_POINT ( 'NONE',  ( 15.60228996708978855, 124.9392590763941371, -1.671781470417840199 ) ) ;
#13577 = CIRCLE ( 'NONE', #3400, 27.69059892324149175 ) ;
#13578 = AXIS2_PLACEMENT_3D ( 'NONE', #4940, #1141, #14425 ) ;
#13579 = CYLINDRICAL_SURFACE ( 'NONE', #10787, 2.500000000000000444 ) ;
#13580 = CARTESIAN_POINT ( 'NONE',  ( 27.48361012698968864, 138.6227766016838245, 1.063447695028166570E-14 ) ) ;
#13581 = AXIS2_PLACEMENT_3D ( 'NONE', #2302, #13101, #6732 ) ;
#13582 = ORIENTED_EDGE ( 'NONE', *, *, #6344, .F. ) ;
#13583 = CARTESIAN_POINT ( 'NONE',  ( 35.00000000000001421, 146.8780590376976249, 21.83693896782702382 ) ) ;
#13584 = VERTEX_POINT ( 'NONE', #15715 ) ;
#13585 = DIRECTION ( 'NONE',  ( 0.000000000000000000, 1.000000000000000000, 0.000000000000000000 ) ) ;
#13586 = CARTESIAN_POINT ( 'NONE',  ( -103.0000000000000142, 171.6227766016838245, 27.69059892324149530 ) ) ;
#13587 = CARTESIAN_POINT ( 'NONE',  ( -100.0000000000000000, 100.0000000000000142, 6.000000000000000000 ) ) ;
#13588 = EDGE_LOOP ( 'NONE', ( #15792, #9415, #14085, #7427, #6683, #6613, #4136, #15497 ) ) ;
#13589 = ORIENTED_EDGE ( 'NONE', *, *, #2452, .F. ) ;
#13590 = AXIS2_PLACEMENT_3D ( 'NONE', #9565, #14972, #15233 ) ;
#13591 = VECTOR ( 'NONE', #15202, 1000.000000000000000 ) ;
#13592 = CARTESIAN_POINT ( 'NONE',  ( 11.28101412774664958, 138.8108036852440250, 13.45198100927934348 ) ) ;
#13593 = CIRCLE ( 'NONE', #15847, 2.500000000000002220 ) ;
#13594 = ORIENTED_EDGE ( 'NONE', *, *, #14950, .F. ) ;
#13595 = SHAPE_DEFINITION_REPRESENTATION ( #16346, #17073 ) ;
#13596 = CARTESIAN_POINT ( 'NONE',  ( 48.00000000000000711, 167.6227766016838530, 5.571800142134975431 ) ) ;
#13597 = DIRECTION ( 'NONE',  ( -0.000000000000000000, -0.000000000000000000, 1.000000000000000000 ) ) ;
#13598 = CARTESIAN_POINT ( 'NONE',  ( 18.93858299686282365, 29.91990340250987757, -11.93041869825017898 ) ) ;
#13599 = EDGE_CURVE ( 'NONE', #9285, #9957, #15417, .T. ) ;
#13600 = DIRECTION ( 'NONE',  ( -0.000000000000000000, -0.000000000000000000, -1.000000000000000000 ) ) ;
#13601 = ADVANCED_FACE ( 'NONE', ( #3767 ), #4917, .F. ) ;
#13602 = CARTESIAN_POINT ( 'NONE',  ( -76.58334154245484626, 150.2902214191207975, 25.17945278758670824 ) ) ;
#13603 = ADVANCED_FACE ( 'NONE', ( #14567 ), #9158, .F. ) ;
#13604 = ORIENTED_EDGE ( 'NONE', *, *, #14950, .T. ) ;
#13605 = DIRECTION ( 'NONE',  ( 0.000000000000000000, 0.000000000000000000, 1.000000000000000000 ) ) ;
#13606 = AXIS2_PLACEMENT_3D ( 'NONE', #13839, #9997, #9741 ) ;
#13607 = CARTESIAN_POINT ( 'NONE',  ( 15.00000000000000000, 143.1210915093834330, -16.64102305613075572 ) ) ;
#13608 = DIRECTION ( 'NONE',  ( -1.000000000000000000, -0.000000000000000000, -0.000000000000000000 ) ) ;
#13609 = DIRECTION ( 'NONE',  ( 0.000000000000000000, 0.000000000000000000, 1.000000000000000000 ) ) ;
#13610 = CARTESIAN_POINT ( 'NONE',  ( 49.99999999999998579, 163.6227766016838530, -10.00000337241049309 ) ) ;
#13611 = VERTEX_POINT ( 'NONE', #10308 ) ;
#13612 = CARTESIAN_POINT ( 'NONE',  ( -100.0000000000000000, 171.6227766016838245, 0.000000000000000000 ) ) ;
#13613 = ORIENTED_EDGE ( 'NONE', *, *, #13863, .T. ) ;
#13614 =( NAMED_UNIT ( * ) SI_UNIT ( $, .STERADIAN. ) SOLID_ANGLE_UNIT ( ) );
#13615 = AXIS2_PLACEMENT_3D ( 'NONE', #10284, #8963, #14374 ) ;
#13616 = VERTEX_POINT ( 'NONE', #3595 ) ;
#13617 =( NAMED_UNIT ( * ) PLANE_ANGLE_UNIT ( ) SI_UNIT ( $, .RADIAN. ) );
#13618 = CARTESIAN_POINT ( 'NONE',  ( 17.58250999373982282, 125.2198453306090045, -5.979920648958140776E-13 ) ) ;
#13619 = PRESENTATION_STYLE_ASSIGNMENT (( #1663 ) ) ;
#13620 = CARTESIAN_POINT ( 'NONE',  ( 27.99999999999998224, 9.999999999999998224, -16.00000000000000000 ) ) ;
#13621 = EDGE_CURVE ( 'NONE', #15447, #7515, #1921, .T. ) ;
#13622 = EDGE_CURVE ( 'NONE', #13560, #2470, #6424, .T. ) ;
#13623 = EDGE_CURVE ( 'NONE', #6848, #1517, #16336, .T. ) ;
#13624 = ORIENTED_EDGE ( 'NONE', *, *, #4524, .T. ) ;
#13625 = DIRECTION ( 'NONE',  ( 0.000000000000000000, 0.000000000000000000, 1.000000000000000000 ) ) ;
#13626 = DIRECTION ( 'NONE',  ( 0.000000000000000000, 0.000000000000000000, -1.000000000000000000 ) ) ;
#13627 = CARTESIAN_POINT ( 'NONE',  ( 14.93242934743711992, 30.00000000000000000, 25.00000000000000000 ) ) ;
#13628 = CARTESIAN_POINT ( 'NONE',  ( -32.64269715136552463, 101.2195121951219647, 4.500000000000000000 ) ) ;
#13629 = DIRECTION ( 'NONE',  ( -1.000000000000000000, 0.000000000000000000, 0.000000000000000000 ) ) ;
#13630 = ORIENTED_EDGE ( 'NONE', *, *, #11695, .T. ) ;
#13631 = CARTESIAN_POINT ( 'NONE',  ( -74.00000000000002842, 146.6227766016838245, -24.49489742783179125 ) ) ;
#13632 = DIRECTION ( 'NONE',  ( -0.000000000000000000, -0.000000000000000000, -1.000000000000000000 ) ) ;
#13633 = VERTEX_POINT ( 'NONE', #13246 ) ;
#13634 = CARTESIAN_POINT ( 'NONE',  ( -45.00000000000000000, 120.0000000000000142, 0.000000000000000000 ) ) ;
#13635 = EDGE_CURVE ( 'NONE', #1799, #16973, #11908, .T. ) ;
#13636 = DIRECTION ( 'NONE',  ( -1.000000000000000000, -0.000000000000000000, 0.000000000000000000 ) ) ;
#13637 = CARTESIAN_POINT ( 'NONE',  ( 31.55028006451160394, 191.8535701216948155, 26.07159546787933024 ) ) ;
#13638 = FACE_OUTER_BOUND ( 'NONE', #14093, .T. ) ;
#13639 = DIRECTION ( 'NONE',  ( 1.000000000000000000, 0.000000000000000000, -0.000000000000000000 ) ) ;
#13640 = CARTESIAN_POINT ( 'NONE',  ( 17.01457324639674695, 29.95810005730942649, 12.72891809691981102 ) ) ;
#13641 = CARTESIAN_POINT ( 'NONE',  ( 15.00000000000903455, 143.2885527162398489, -16.91661185963483760 ) ) ;
#13642 = EDGE_LOOP ( 'NONE', ( #6130, #16908 ) ) ;
#13643 = CARTESIAN_POINT ( 'NONE',  ( -25.81900932159183526, 19.99999999999999645, -13.95463872937544991 ) ) ;
#13644 = ORIENTED_EDGE ( 'NONE', *, *, #12902, .T. ) ;
#13645 = FACE_OUTER_BOUND ( 'NONE', #13076, .T. ) ;
#13646 = DIRECTION ( 'NONE',  ( 1.000000000000000000, -0.000000000000000000, -0.000000000000000000 ) ) ;
#13647 = ORIENTED_EDGE ( 'NONE', *, *, #10200, .T. ) ;
#13648 = CARTESIAN_POINT ( 'NONE',  ( -3.000000000000000888, 154.3022685259950038, 9.999999999999900524 ) ) ;
#13649 = CARTESIAN_POINT ( 'NONE',  ( -74.00000000000002842, 146.6227766016838245, -16.00000000000000000 ) ) ;
#13650 = ORIENTED_EDGE ( 'NONE', *, *, #9927, .F. ) ;
#13651 = PRODUCT_DEFINITION_SHAPE ( 'NONE', 'NONE',  #3279 ) ;
#13652 = CARTESIAN_POINT ( 'NONE',  ( 23.19504936680528573, 149.8103701614163015, -24.76910924193868979 ) ) ;
#13653 = ADVANCED_FACE ( 'NONE', ( #17314 ), #6327, .T. ) ;
#13654 = ORIENTED_EDGE ( 'NONE', *, *, #5271, .F. ) ;
#13655 = CARTESIAN_POINT ( 'NONE',  ( -21.99999999999998579, 10.00000000000000000, -30.00000000000000355 ) ) ;
#13656 = PLANE ( 'NONE',  #5791 ) ;
#13657 = CARTESIAN_POINT ( 'NONE',  ( -27.99999999999998224, 10.00000000000000000, -16.00000000000000000 ) ) ;
#13658 = VERTEX_POINT ( 'NONE', #10233 ) ;
#13659 = DIRECTION ( 'NONE',  ( 0.000000000000000000, 0.000000000000000000, 1.000000000000000000 ) ) ;
#13660 = ADVANCED_FACE ( 'NONE', ( #17221 ), #13807, .F. ) ;
#13661 = EDGE_CURVE ( 'NONE', #11634, #12789, #15809, .T. ) ;
#13662 = ORIENTED_EDGE ( 'NONE', *, *, #9391, .T. ) ;
#13663 = CARTESIAN_POINT ( 'NONE',  ( 35.00000000000000711, 146.6227766016838245, 21.54065922853802562 ) ) ;
#13664 = APPLICATION_CONTEXT ( 'automotive_design' ) ;
#13665 = ORIENTED_EDGE ( 'NONE', *, *, #12360, .T. ) ;
#13666 = LINE ( 'NONE', #4107, #5062 ) ;
#13667 = DIRECTION ( 'NONE',  ( 8.673617379884037937E-17, 0.000000000000000000, -1.000000000000000000 ) ) ;
#13668 = ORIENTED_EDGE ( 'NONE', *, *, #7974, .T. ) ;
#13669 = VERTEX_POINT ( 'NONE', #14660 ) ;
#13670 = VERTEX_POINT ( 'NONE', #15631 ) ;
#13671 = CARTESIAN_POINT ( 'NONE',  ( -206.3689767832464668, 173.6103877383153531, -4.531616471133038004 ) ) ;
#13672 = LINE ( 'NONE', #14741, #10681 ) ;
#13673 = ORIENTED_EDGE ( 'NONE', *, *, #11223, .F. ) ;
#13674 = APPLICATION_PROTOCOL_DEFINITION ( 'draft international standard', 'automotive_design', 1998, #12523 ) ;
#13675 = LINE ( 'NONE', #5363, #3134 ) ;
#13676 = DIRECTION ( 'NONE',  ( 1.000000000000000000, 0.000000000000000000, 0.000000000000000000 ) ) ;
#13677 = FACE_OUTER_BOUND ( 'NONE', #6821, .T. ) ;
#13678 = DIRECTION ( 'NONE',  ( -1.000000000000000000, 0.000000000000000000, 0.000000000000000000 ) ) ;
#13679 = CARTESIAN_POINT ( 'NONE',  ( -75.93727504753279334, 149.5415222133261182, 24.52446659945425367 ) ) ;
#13680 = ORIENTED_EDGE ( 'NONE', *, *, #9737, .F. ) ;
#13681 = CARTESIAN_POINT ( 'NONE',  ( -77.38716036884935079, 202.0279528788175583, -17.33673759440342010 ) ) ;
#13682 = DIRECTION ( 'NONE',  ( 1.000000000000000000, 6.217248937900877415E-15, 0.000000000000000000 ) ) ;
#13683 = DIRECTION ( 'NONE',  ( -1.000000000000000000, -0.000000000000000000, -0.000000000000000000 ) ) ;
#13684 = AXIS2_PLACEMENT_3D ( 'NONE', #13873, #13683, #15274 ) ;
#13685 = CARTESIAN_POINT ( 'NONE',  ( -34.99999999999999289, 122.0000000000000284, -4.999999999999999112 ) ) ;
#13686 = DIRECTION ( 'NONE',  ( 0.000000000000000000, 1.850371707708594563E-16, 1.000000000000000000 ) ) ;
#13687 = UNCERTAINTY_MEASURE_WITH_UNIT (LENGTH_MEASURE( 1.000000000000000082E-05 ), #15973, 'distance_accuracy_value', 'NONE');
#13688 = EDGE_LOOP ( 'NONE', ( #17302, #2203, #4171, #104, #9398 ) ) ;
#13689 = LINE ( 'NONE', #11032, #862 ) ;
#13690 = ADVANCED_FACE ( 'NONE', ( #771, #12896 ), #3509, .T. ) ;
#13691 = EDGE_LOOP ( 'NONE', ( #10241, #4311, #3453, #1884 ) ) ;
#13692 = ORIENTED_EDGE ( 'NONE', *, *, #13208, .T. ) ;
#13693 = CARTESIAN_POINT ( 'NONE',  ( -15.00000000000001421, 19.99999999999995737, 13.00000000000000000 ) ) ;
#13694 = SURFACE_STYLE_FILL_AREA ( #8288 ) ;
#13695 = AXIS2_PLACEMENT_3D ( 'NONE', #8538, #3487, #7460 ) ;
#13696 = CARTESIAN_POINT ( 'NONE',  ( -27.98221281347037603, 18.00000000000000000, 0.000000000000000000 ) ) ;
#13697 = AXIS2_PLACEMENT_3D ( 'NONE', #3969, #14020, #9671 ) ;
#13698 = EDGE_LOOP ( 'NONE', ( #15969, #434, #5708, #269 ) ) ;
#13699 = DIRECTION ( 'NONE',  ( 1.000000000000000000, 0.000000000000000000, 0.000000000000000000 ) ) ;
#13700 = CARTESIAN_POINT ( 'NONE',  ( -32.64269715136551753, 101.2195121951219647, 5.500000000000000000 ) ) ;
#13701 = DIRECTION ( 'NONE',  ( 0.000000000000000000, 0.000000000000000000, -1.000000000000000000 ) ) ;
#13702 = CARTESIAN_POINT ( 'NONE',  ( 48.00000000000000711, 191.6227766016837677, 5.571800142134975431 ) ) ;
#13703 = AXIS2_PLACEMENT_3D ( 'NONE', #17449, #5673, #13722 ) ;
#13704 = CARTESIAN_POINT ( 'NONE',  ( 23.14977753070778377, 139.1449216839932319, -13.05325656350955654 ) ) ;
#13705 = EDGE_CURVE ( 'NONE', #14253, #5417, #11813, .T. ) ;
#13706 = EDGE_CURVE ( 'NONE', #10977, #3421, #12952, .T. ) ;
#13707 = AXIS2_PLACEMENT_3D ( 'NONE', #11909, #13071, #17315 ) ;
#13708 = ADVANCED_FACE ( 'NONE', ( #3960, #4217 ), #16083, .F. ) ;
#13709 = VERTEX_POINT ( 'NONE', #1289 ) ;
#13710 = CARTESIAN_POINT ( 'NONE',  ( -75.69074982301630428, 150.8166157800934002, -28.14689102807276200 ) ) ;
#13711 = CARTESIAN_POINT ( 'NONE',  ( 15.22098041563561388, 126.0279773824920824, -6.884464680362713196 ) ) ;
#13712 = ORIENTED_EDGE ( 'NONE', *, *, #16168, .F. ) ;
#13713 = CARTESIAN_POINT ( 'NONE',  ( -79.53915657140119322, 190.6362156748385530, -29.38520182610347575 ) ) ;
#13714 = DIRECTION ( 'NONE',  ( 1.000000000000000000, 0.000000000000000000, -0.000000000000000000 ) ) ;
#13715 = CARTESIAN_POINT ( 'NONE',  ( 29.02955226949582368, 191.7140209832038238, 26.17909706909631851 ) ) ;
#13717 = PLANE ( 'NONE',  #7259 ) ;
#13716 = B_SPLINE_CURVE_WITH_KNOTS ( 'NONE', 3,
 ( #5855, #13738, #13922, #5952 ),
 .UNSPECIFIED., .F., .F.,
 ( 4, 4 ),
 ( 0.001580575003448743973, 0.001893147295999755278 ),
 .UNSPECIFIED. ) ;
#13718 = CIRCLE ( 'NONE', #15976, 7.500000000000000000 ) ;
#13719 = DIRECTION ( 'NONE',  ( 0.000000000000000000, 0.000000000000000000, -1.000000000000000000 ) ) ;
#13720 = CARTESIAN_POINT ( 'NONE',  ( -15.00000000000001421, 20.00000000000004263, -4.999999999999999112 ) ) ;
#13721 = AXIS2_PLACEMENT_3D ( 'NONE', #13535, #10600, #6447 ) ;
#13722 = DIRECTION ( 'NONE',  ( 1.000000000000000000, 0.000000000000000000, 0.000000000000000000 ) ) ;
#13723 = AXIS2_PLACEMENT_3D ( 'NONE', #12226, #97, #1248 ) ;
#13724 = PLANE ( 'NONE',  #15408 ) ;
#13725 = ORIENTED_EDGE ( 'NONE', *, *, #13440, .F. ) ;
#13726 = CARTESIAN_POINT ( 'NONE',  ( -10.00647404944701258, 19.99999999999999645, -14.03129316391565951 ) ) ;
#13727 = ORIENTED_EDGE ( 'NONE', *, *, #8958, .T. ) ;
#13728 = CARTESIAN_POINT ( 'NONE',  ( -208.3486229709906468, 168.0754701982165500, 6.144114920819691683 ) ) ;
#13729 = DIRECTION ( 'NONE',  ( 0.000000000000000000, 0.000000000000000000, -1.000000000000000000 ) ) ;
#13730 = EDGE_LOOP ( 'NONE', ( #14675, #10133, #17158, #5082, #15403 ) ) ;
#13731 = CARTESIAN_POINT ( 'NONE',  ( -15.33310217279680288, 19.99999999999999645, 4.999999999999999112 ) ) ;
#13732 = DIRECTION ( 'NONE',  ( 0.000000000000000000, 0.000000000000000000, 1.000000000000000000 ) ) ;
#13733 =( GEOMETRIC_REPRESENTATION_CONTEXT ( 3 ) GLOBAL_UNCERTAINTY_ASSIGNED_CONTEXT ( ( #2424 ) ) GLOBAL_UNIT_ASSIGNED_CONTEXT ( ( #9338, #2260, #6247 ) ) REPRESENTATION_CONTEXT ( 'NONE', 'WORKASPACE' ) );
#13734 = ORIENTED_EDGE ( 'NONE', *, *, #302, .F. ) ;
#13735 = AXIS2_PLACEMENT_3D ( 'NONE', #6524, #9168, #9080 ) ;
#13736 = CARTESIAN_POINT ( 'NONE',  ( 30.59986690501726514, 154.1043103600818540, -27.96613953460096269 ) ) ;
#13737 = AXIS2_PLACEMENT_3D ( 'NONE', #2043, #3194, #10261 ) ;
#13738 = CARTESIAN_POINT ( 'NONE',  ( -32.66708739526796279, 101.0743296803272386, -4.648821459077780993 ) ) ;
#13739 = CARTESIAN_POINT ( 'NONE',  ( 0.000000000000000000, 2.000000000000000000, 0.000000000000000000 ) ) ;
#13740 = CARTESIAN_POINT ( 'NONE',  ( -23.00000000000000000, 120.0000000000000284, 4.999999999999999112 ) ) ;
#13741 = LINE ( 'NONE', #12416, #6260 ) ;
#13742 = ORIENTED_EDGE ( 'NONE', *, *, #741, .T. ) ;
#13743 = CARTESIAN_POINT ( 'NONE',  ( -27.99999999999998224, 10.00000000000000000, -35.00200000000000244 ) ) ;
#13744 = AXIS2_PLACEMENT_3D ( 'NONE', #1886, #12947, #1974 ) ;
#13745 = CARTESIAN_POINT ( 'NONE',  ( 25.00000000000000711, 146.6227766016838245, 21.54065922853802562 ) ) ;
#13746 = CIRCLE ( 'NONE', #16003, 33.00000000000000000 ) ;
#13747 = ORIENTED_EDGE ( 'NONE', *, *, #1129, .T. ) ;
#13748 = CARTESIAN_POINT ( 'NONE',  ( 18.97648483518030815, 140.5725221174451747, -16.15500418213391143 ) ) ;
#13749 = EDGE_CURVE ( 'NONE', #12276, #4284, #17500, .T. ) ;
#13750 = CIRCLE ( 'NONE', #10905, 19.49999999999998934 ) ;
#13751 = VERTEX_POINT ( 'NONE', #6949 ) ;
#13752 = ADVANCED_FACE ( 'NONE', ( #4302 ), #135, .F. ) ;
#13753 = LINE ( 'NONE', #16765, #2512 ) ;
#13754 = CARTESIAN_POINT ( 'NONE',  ( -68.00000000000000000, 171.6227766016838245, 0.000000000000000000 ) ) ;
#13755 = CARTESIAN_POINT ( 'NONE',  ( -10.05738114656989346, 30.87167111307020306, -12.65386873594253103 ) ) ;
#13756 = VERTEX_POINT ( 'NONE', #12089 ) ;
#13757 = ORIENTED_EDGE ( 'NONE', *, *, #3571, .F. ) ;
#13758 = CARTESIAN_POINT ( 'NONE',  ( 48.00000000000000711, 151.6227766016839098, 5.571800142134973655 ) ) ;
#13759 = CARTESIAN_POINT ( 'NONE',  ( 17.56954167074719919, 125.3114906870353167, 3.338394383324010395 ) ) ;
#13760 = CARTESIAN_POINT ( 'NONE',  ( 18.30724418481576166, 140.7653321920888345, 16.52022657272140904 ) ) ;
#13761 = EDGE_CURVE ( 'NONE', #8849, #2293, #1, .T. ) ;
#13762 = AXIS2_PLACEMENT_3D ( 'NONE', #5421, #16223, #11145 ) ;
#13763 = CIRCLE ( 'NONE', #12061, 4.999999999999997335 ) ;
#13764 = ORIENTED_EDGE ( 'NONE', *, *, #16931, .T. ) ;
#13765 = APPLICATION_PROTOCOL_DEFINITION ( 'draft international standard', 'automotive_design', 1998, #9124 ) ;
#13766 = DIRECTION ( 'NONE',  ( 0.000000000000000000, 1.000000000000000000, 0.000000000000000000 ) ) ;
#13767 = CIRCLE ( 'NONE', #3582, 5.000000000000007994 ) ;
#13768 = DIRECTION ( 'NONE',  ( 0.000000000000000000, 0.000000000000000000, -1.000000000000000000 ) ) ;
#13769 = CIRCLE ( 'NONE', #9518, 5.999999999999998224 ) ;
#13770 = CARTESIAN_POINT ( 'NONE',  ( 14.93242934743710393, 30.00000000000000000, -13.00000000000000178 ) ) ;
#13771 = CARTESIAN_POINT ( 'NONE',  ( -33.00000000000000711, 171.6227766016838245, 0.000000000000000000 ) ) ;
#13772 = CYLINDRICAL_SURFACE ( 'NONE', #13485, 2.500000000000000444 ) ;
#13773 = ORIENTED_EDGE ( 'NONE', *, *, #3323, .F. ) ;
#13774 = CARTESIAN_POINT ( 'NONE',  ( -32.65377812985507688, 100.8098204658883645, 4.906772862994293050 ) ) ;
#13775 = DIRECTION ( 'NONE',  ( -0.000000000000000000, -0.000000000000000000, 1.000000000000000000 ) ) ;
#13776 = CARTESIAN_POINT ( 'NONE',  ( 17.55923266082603007, 19.99999999999999645, -24.87049340120105612 ) ) ;
#13777 = EDGE_CURVE ( 'NONE', #8027, #5427, #515, .T. ) ;
#13778 = CARTESIAN_POINT ( 'NONE',  ( -40.00000000000000711, 0.000000000000000000, 0.000000000000000000 ) ) ;
#13779 = CARTESIAN_POINT ( 'NONE',  ( 40.00000000000000711, 136.6227766016838245, 0.000000000000000000 ) ) ;
#13780 = VERTEX_POINT ( 'NONE', #3049 ) ;
#13781 = AXIS2_PLACEMENT_3D ( 'NONE', #4005, #1240, #2150 ) ;
#13782 = ORIENTED_EDGE ( 'NONE', *, *, #16757, .T. ) ;
#13783 = PRESENTATION_LAYER_ASSIGNMENT (  '', '', ( #13501 ) ) ;
#13784 = MECHANICAL_DESIGN_GEOMETRIC_PRESENTATION_REPRESENTATION (  '', ( #14076 ), #8117 ) ;
#13785 = EDGE_CURVE ( 'NONE', #9691, #10464, #3146, .T. ) ;
#13786 = DIRECTION ( 'NONE',  ( 0.000000000000000000, -0.8660254037844413721, -0.4999999999999953371 ) ) ;
#13787 = EDGE_LOOP ( 'NONE', ( #5039, #9432, #16942, #16503 ) ) ;
#13788 = EDGE_CURVE ( 'NONE', #10037, #8931, #13950, .T. ) ;
#13789 = DIRECTION ( 'NONE',  ( 0.000000000000000000, 0.000000000000000000, -1.000000000000000000 ) ) ;
#13790 = EDGE_CURVE ( 'NONE', #5589, #1310, #14932, .T. ) ;
#13791 = EDGE_LOOP ( 'NONE', ( #12451, #9982 ) ) ;
#13792 =( NAMED_UNIT ( * ) PLANE_ANGLE_UNIT ( ) SI_UNIT ( $, .RADIAN. ) );
#13793 = DIRECTION ( 'NONE',  ( -1.000000000000000000, 0.000000000000000000, 0.000000000000000000 ) ) ;
#13794 = DIRECTION ( 'NONE',  ( -1.000000000000000000, 0.000000000000000000, 0.000000000000000000 ) ) ;
#13795 = DIRECTION ( 'NONE',  ( 0.000000000000000000, 0.000000000000000000, -1.000000000000000000 ) ) ;
#13796 = CARTESIAN_POINT ( 'NONE',  ( -27.98221281347037959, 20.00000000000000000, -4.999999999999999112 ) ) ;
#13797 = AXIS2_PLACEMENT_3D ( 'NONE', #5470, #13625, #16370 ) ;
#13798 = AXIS2_PLACEMENT_3D ( 'NONE', #127, #16247, #2699 ) ;
#13799 = AXIS2_PLACEMENT_3D ( 'NONE', #2080, #8816, #12802 ) ;
#13800 = EDGE_LOOP ( 'NONE', ( #4532, #16705 ) ) ;
#13801 = CARTESIAN_POINT ( 'NONE',  ( 49.99999999999998579, 175.6227766016838245, 5.571800142134975431 ) ) ;
#13802 = CARTESIAN_POINT ( 'NONE',  ( 48.00000000000000711, 151.6227766016839098, -3.071800142134974099 ) ) ;
#13803 = EDGE_CURVE ( 'NONE', #4701, #13081, #11528, .T. ) ;
#13804 = LINE ( 'NONE', #8743, #16136 ) ;
#13805 = CARTESIAN_POINT ( 'NONE',  ( -95.00000000000000000, 143.9321776784423150, 5.086680500673126297E-15 ) ) ;
#13806 = CARTESIAN_POINT ( 'NONE',  ( 16.97810798871989135, 126.5456571586929044, -7.842726245482330327 ) ) ;
#13807 = CONICAL_SURFACE ( 'NONE', #6165, 2.500000000000002220, 1.029744260000002631 ) ;
#13808 = VERTEX_POINT ( 'NONE', #1995 ) ;
#13809 = DIRECTION ( 'NONE',  ( 1.000000000000000000, 0.000000000000000000, -0.000000000000000000 ) ) ;
#13810 = AXIS2_PLACEMENT_3D ( 'NONE', #5045, #14607, #6733 ) ;
#13811 = STYLED_ITEM ( 'NONE', ( #1843 ), #14383 ) ;
#13812 = CARTESIAN_POINT ( 'NONE',  ( 14.16484689353800697, 138.6662281288708982, -3.797024489650347334 ) ) ;
#13813 = ORIENTED_EDGE ( 'NONE', *, *, #10094, .T. ) ;
#13814 = CARTESIAN_POINT ( 'NONE',  ( -74.00000000000001421, 196.6227766016838245, -24.49489742783179125 ) ) ;
#13815 = CYLINDRICAL_SURFACE ( 'NONE', #1935, 5.000000000000004441 ) ;
#13816 = DIRECTION ( 'NONE',  ( 0.000000000000000000, 0.000000000000000000, 1.000000000000000000 ) ) ;
#13817 = FACE_BOUND ( 'NONE', #10783, .T. ) ;
#13818 = CYLINDRICAL_SURFACE ( 'NONE', #3885, 2.499999999999998668 ) ;
#13819 = CARTESIAN_POINT ( 'NONE',  ( -43.00000000000000711, 130.0000000000000000, 12.99999999999999822 ) ) ;
#13820 = EDGE_CURVE ( 'NONE', #12853, #6658, #5887, .T. ) ;
#13821 = EDGE_CURVE ( 'NONE', #2935, #539, #12791, .T. ) ;
#13822 = AXIS2_PLACEMENT_3D ( 'NONE', #15416, #4630, #8601 ) ;
#13823 = CARTESIAN_POINT ( 'NONE',  ( -82.96816024544703794, 200.6580771142793651, 15.68801935549125481 ) ) ;
#13824 = EDGE_CURVE ( 'NONE', #4320, #805, #7572, .T. ) ;
#13825 = AXIS2_PLACEMENT_3D ( 'NONE', #13620, #8376, #4319 ) ;
#13826 = FACE_OUTER_BOUND ( 'NONE', #13474, .T. ) ;
#13827 = ORIENTED_EDGE ( 'NONE', *, *, #12324, .T. ) ;
#13828 = ORIENTED_EDGE ( 'NONE', *, *, #15816, .T. ) ;
#13829 = LINE ( 'NONE', #8411, #14289 ) ;
#13830 = FACE_OUTER_BOUND ( 'NONE', #4942, .T. ) ;
#13831 = ORIENTED_EDGE ( 'NONE', *, *, #17458, .T. ) ;
#13832 = CARTESIAN_POINT ( 'NONE',  ( -17.11671918504270451, 32.08177433558115865, 9.477319364664337442 ) ) ;
#13833 = DIRECTION ( 'NONE',  ( 1.000000000000000000, -0.000000000000000000, -0.000000000000000000 ) ) ;
#13834 = AXIS2_PLACEMENT_3D ( 'NONE', #16131, #10532, #5490 ) ;
#13835 = VERTEX_POINT ( 'NONE', #2962 ) ;
#13836 = AXIS2_PLACEMENT_3D ( 'NONE', #1389, #13609, #4220 ) ;
#13837 = CARTESIAN_POINT ( 'NONE',  ( 37.50000000000000711, 196.6227766016838245, -21.54065922853802562 ) ) ;
#13838 = VECTOR ( 'NONE', #3956, 1000.000000000000000 ) ;
#13839 = CARTESIAN_POINT ( 'NONE',  ( 27.99999999999998224, 9.999999999999998224, 35.00200000000000244 ) ) ;
#13840 = CARTESIAN_POINT ( 'NONE',  ( -207.7491074081026170, 166.3381691538542384, -1.234337273009209701 ) ) ;
#13841 = DIRECTION ( 'NONE',  ( -1.000000000000000000, -0.000000000000000000, -0.000000000000000000 ) ) ;
#13842 = CARTESIAN_POINT ( 'NONE',  ( -68.00000000000000000, 171.6227766016838245, 0.000000000000000000 ) ) ;
#13843 = EDGE_CURVE ( 'NONE', #15544, #2395, #10029, .T. ) ;
#13844 = CARTESIAN_POINT ( 'NONE',  ( -138.7106781186547266, 171.6227766016838245, -25.00000000000000000 ) ) ;
#13845 = CARTESIAN_POINT ( 'NONE',  ( -70.00000000000000000, 206.6227766016838245, -2.143131898507868248E-15 ) ) ;
#13846 = ORIENTED_EDGE ( 'NONE', *, *, #1296, .T. ) ;
#13847 = FACE_BOUND ( 'NONE', #11323, .T. ) ;
#13848 = TOROIDAL_SURFACE ( 'NONE', #10725, 14.16444493696511486, 5.000000000000000000 ) ;
#13849 = VECTOR ( 'NONE', #15597, 1000.000000000000000 ) ;
#13850 = ORIENTED_EDGE ( 'NONE', *, *, #6319, .F. ) ;
#13851 = DIRECTION ( 'NONE',  ( 0.000000000000000000, 0.000000000000000000, -1.000000000000000000 ) ) ;
#13852 = AXIS2_PLACEMENT_3D ( 'NONE', #7611, #16752, #896 ) ;
#13853 = LINE ( 'NONE', #9757, #14029 ) ;
#13854 = ORIENTED_EDGE ( 'NONE', *, *, #14670, .F. ) ;
#13855 = ORIENTED_EDGE ( 'NONE', *, *, #12360, .F. ) ;
#13856 = DIRECTION ( 'NONE',  ( -0.000000000000000000, -0.000000000000000000, -1.000000000000000000 ) ) ;
#13857 = CARTESIAN_POINT ( 'NONE',  ( 2.750000000000000000, 0.000000000000000000, 2.699999999999999289 ) ) ;
#13858 = CARTESIAN_POINT ( 'NONE',  ( 15.33542211484438056, 137.4551579351393400, 9.454295640946218882 ) ) ;
#13859 = AXIS2_PLACEMENT_3D ( 'NONE', #4179, #2927, #13732 ) ;
#13860 = VECTOR ( 'NONE', #14790, 1000.000000000000000 ) ;
#13861 = EDGE_LOOP ( 'NONE', ( #2098, #8647, #3488, #8675 ) ) ;
#13862 = LINE ( 'NONE', #571, #5402 ) ;
#13863 = EDGE_CURVE ( 'NONE', #1718, #6730, #3389, .T. ) ;
#13864 = VECTOR ( 'NONE', #5139, 1000.000000000000000 ) ;
#13865 = DIRECTION ( 'NONE',  ( 0.9961946980917461003, -0.04357787137382522491, -0.07547908730516825204 ) ) ;
#13866 = DIRECTION ( 'NONE',  ( 1.000000000000000000, -0.000000000000000000, 0.000000000000000000 ) ) ;
#13867 = LINE ( 'NONE', #7040, #9070 ) ;
#13868 = DIRECTION ( 'NONE',  ( -1.000000000000000000, -0.000000000000000000, -0.000000000000000000 ) ) ;
#13869 = LINE ( 'NONE', #4384, #15379 ) ;
#13870 = ORIENTED_EDGE ( 'NONE', *, *, #6657, .T. ) ;
#13871 = CARTESIAN_POINT ( 'NONE',  ( -32.14917720409751922, 100.1152149123505382, 5.472305571546616676 ) ) ;
#13872 = DIRECTION ( 'NONE',  ( -1.000000000000000000, 0.000000000000000000, 0.000000000000000000 ) ) ;
#13873 = CARTESIAN_POINT ( 'NONE',  ( 196.0000000000000000, 175.6227766016838530, 19.42820660268601074 ) ) ;
#13874 = CARTESIAN_POINT ( 'NONE',  ( 48.00000000000000711, 167.6227766016838814, -19.42820660268601074 ) ) ;
#13875 = DIRECTION ( 'NONE',  ( -0.000000000000000000, -0.000000000000000000, 1.000000000000000000 ) ) ;
#13876 = AXIS2_PLACEMENT_3D ( 'NONE', #16450, #16183, #6799 ) ;
#13877 = AXIS2_PLACEMENT_3D ( 'NONE', #9801, #16542, #13895 ) ;
#13878 = ORIENTED_EDGE ( 'NONE', *, *, #1296, .F. ) ;
#13879 = EDGE_LOOP ( 'NONE', ( #16791, #2374 ) ) ;
#13880 = AXIS2_PLACEMENT_3D ( 'NONE', #14477, #17214, #5091 ) ;
#13881 = CARTESIAN_POINT ( 'NONE',  ( 11.58137902169841027, 143.8440485058968363, 17.81491816053495825 ) ) ;
#13882 = ORIENTED_EDGE ( 'NONE', *, *, #279, .T. ) ;
#13883 = SURFACE_STYLE_USAGE ( .BOTH. , #11382 ) ;
#13884 = VERTEX_POINT ( 'NONE', #3226 ) ;
#13885 = DIRECTION ( 'NONE',  ( 0.000000000000000000, 0.000000000000000000, 1.000000000000000000 ) ) ;
#13886 = EDGE_CURVE ( 'NONE', #2002, #12276, #16065, .T. ) ;
#13887 = FILL_AREA_STYLE_COLOUR ( '', #17110 ) ;
#13888 = CARTESIAN_POINT ( 'NONE',  ( -155.0000000000000284, 171.6227766016838245, 21.61734737250326077 ) ) ;
#13889 = AXIS2_PLACEMENT_3D ( 'NONE', #1646, #13775, #2964 ) ;
#13890 = DIRECTION ( 'NONE',  ( 1.000000000000000000, 0.000000000000000000, 0.000000000000000000 ) ) ;
#13891 = CARTESIAN_POINT ( 'NONE',  ( 33.88365274872860766, 18.00000000000000000, -11.43011099234507277 ) ) ;
#13892 = EDGE_LOOP ( 'NONE', ( #2120, #825, #9104, #8454 ) ) ;
#13893 = CARTESIAN_POINT ( 'NONE',  ( 34.97205211421869819, 146.0169975363979802, 20.82225907110314012 ) ) ;
#13894 = DIRECTION ( 'NONE',  ( -1.000000000000000000, -0.000000000000000000, -0.000000000000000000 ) ) ;
#13895 = DIRECTION ( 'NONE',  ( 0.000000000000000000, 0.000000000000000000, 1.000000000000000000 ) ) ;
#13896 = EDGE_CURVE ( 'NONE', #3475, #4586, #9710, .T. ) ;
#13897 = CARTESIAN_POINT ( 'NONE',  ( -40.00000000000000000, 0.000000000000000000, 33.00000000000000711 ) ) ;
#13898 = ADVANCED_FACE ( 'NONE', ( #5716 ), #14645, .F. ) ;
#13899 = VECTOR ( 'NONE', #2957, 1000.000000000000000 ) ;
#13900 = DIRECTION ( 'NONE',  ( 0.000000000000000000, 0.000000000000000000, 1.000000000000000000 ) ) ;
#13901 = ORIENTED_EDGE ( 'NONE', *, *, #2622, .F. ) ;
#13902 = CARTESIAN_POINT ( 'NONE',  ( 49.99999999999998579, 151.6227766016839098, -5.571800142134973655 ) ) ;
#13903 = VERTEX_POINT ( 'NONE', #8966 ) ;
#13904 = CARTESIAN_POINT ( 'NONE',  ( -78.86396916296997972, 190.7269353522202664, -29.32635129980144839 ) ) ;
#13905 = CARTESIAN_POINT ( 'NONE',  ( 27.99999999999998224, 9.999999999999998224, 35.00200000000000244 ) ) ;
#13906 = DIRECTION ( 'NONE',  ( 0.000000000000000000, 1.000000000000000000, 0.000000000000000000 ) ) ;
#13907 = FACE_OUTER_BOUND ( 'NONE', #3189, .T. ) ;
#13908 = DIRECTION ( 'NONE',  ( -0.08715574274764653628, -0.4980973490458781017, 0.8627299156628190913 ) ) ;
#13909 = FACE_OUTER_BOUND ( 'NONE', #13588, .T. ) ;
#13910 = CARTESIAN_POINT ( 'NONE',  ( -85.00000000000002842, 196.6227766016838245, 21.54065922853802562 ) ) ;
#13911 = FACE_BOUND ( 'NONE', #332, .T. ) ;
#13912 = VERTEX_POINT ( 'NONE', #2328 ) ;
#13913 = ORIENTED_EDGE ( 'NONE', *, *, #8406, .T. ) ;
#13914 = CARTESIAN_POINT ( 'NONE',  ( 48.00000000000000711, 163.6227766016838530, 12.50000337241049309 ) ) ;
#13915 = CARTESIAN_POINT ( 'NONE',  ( 49.99999999999998579, 175.6227766016838530, -21.92820660268601074 ) ) ;
#13916 = ORIENTED_EDGE ( 'NONE', *, *, #3678, .T. ) ;
#13917 = CARTESIAN_POINT ( 'NONE',  ( -26.11264420168842904, 19.99999999999999645, 13.35921939055851482 ) ) ;
#13918 = DIRECTION ( 'NONE',  ( 1.000000000000000000, 0.000000000000000000, 0.000000000000000000 ) ) ;
#13919 = EDGE_LOOP ( 'NONE', ( #4970, #5199, #4158, #8866 ) ) ;
#13920 = ADVANCED_FACE ( 'NONE', ( #6231 ), #17200, .F. ) ;
#13921 = FACE_OUTER_BOUND ( 'NONE', #7601, .T. ) ;
#13922 = CARTESIAN_POINT ( 'NONE',  ( -32.65876937324905072, 101.1480800978618362, -4.574127464407660604 ) ) ;
#13923 = CARTESIAN_POINT ( 'NONE',  ( -208.1430079281944074, 166.0913325906388422, -2.284806080016993590 ) ) ;
#13924 = LINE ( 'NONE', #3201, #16266 ) ;
#13925 = CARTESIAN_POINT ( 'NONE',  ( -208.0000000000000853, 174.7326106162513497, 53.79077198841061147 ) ) ;
#13926 = CARTESIAN_POINT ( 'NONE',  ( 0.000000000000000000, 5.817072295949927426E-16, -4.750000000000000000 ) ) ;
#13927 = DIRECTION ( 'NONE',  ( -0.000000000000000000, -0.000000000000000000, 1.000000000000000000 ) ) ;
#13928 = ORIENTED_EDGE ( 'NONE', *, *, #15837, .T. ) ;
#13929 = CARTESIAN_POINT ( 'NONE',  ( 21.93446201513734550, 139.6105936900751203, -14.17700481206107455 ) ) ;
#13930 = VERTEX_POINT ( 'NONE', #7720 ) ;
#13931 = LINE ( 'NONE', #3392, #1107 ) ;
#13932 = CARTESIAN_POINT ( 'NONE',  ( -13.22984127103138796, 31.85746429949665881, -11.06592603413638898 ) ) ;
#13933 = EDGE_LOOP ( 'NONE', ( #147, #4823, #3495 ) ) ;
#13934 = EDGE_LOOP ( 'NONE', ( #16347, #963 ) ) ;
#13935 = DIRECTION ( 'NONE',  ( -1.000000000000000000, -0.000000000000000000, -0.000000000000000000 ) ) ;
#13936 = EDGE_CURVE ( 'NONE', #1055, #7056, #16640, .T. ) ;
#13937 = EDGE_CURVE ( 'NONE', #16675, #11660, #5323, .T. ) ;
#13938 = CARTESIAN_POINT ( 'NONE',  ( -45.00000000000000000, 134.2062027339443944, -15.00000000000000000 ) ) ;
#13939 = EDGE_CURVE ( 'NONE', #14899, #15553, #17482, .T. ) ;
#13940 = CARTESIAN_POINT ( 'NONE',  ( 21.84350049701297536, 139.6359888969276426, 14.21326463380156646 ) ) ;
#13941 = EDGE_LOOP ( 'NONE', ( #16441, #8118 ) ) ;
#13942 = CONTEXT_DEPENDENT_SHAPE_REPRESENTATION ( #3603, #10119 ) ;
#13943 = DIRECTION ( 'NONE',  ( 1.000000000000000000, 0.000000000000000000, 0.000000000000000000 ) ) ;
#13944 = DIRECTION ( 'NONE',  ( 1.000000000000000000, 0.000000000000000000, -0.000000000000000000 ) ) ;
#13945 = CARTESIAN_POINT ( 'NONE',  ( -85.00000000000002842, 196.6227766016838245, 21.54065922853802562 ) ) ;
#13946 = DIRECTION ( 'NONE',  ( -1.000000000000000000, -0.000000000000000000, 0.000000000000000000 ) ) ;
#13947 = CARTESIAN_POINT ( 'NONE',  ( 24.93034343272520204, 18.00000000000000000, 22.33460256651928333 ) ) ;
#13948 = DIRECTION ( 'NONE',  ( 0.000000000000000000, 0.000000000000000000, 1.000000000000000000 ) ) ;
#13949 = ORIENTED_EDGE ( 'NONE', *, *, #14249, .F. ) ;
#13950 = LINE ( 'NONE', #14128, #16363 ) ;
#13951 = FACE_OUTER_BOUND ( 'NONE', #8431, .T. ) ;
#13952 = DIRECTION ( 'NONE',  ( -0.000000000000000000, -0.000000000000000000, -1.000000000000000000 ) ) ;
#13953 = CARTESIAN_POINT ( 'NONE',  ( 30.00000000000001066, 146.6227766016838245, -16.00000000000000000 ) ) ;
#13954 = DIRECTION ( 'NONE',  ( 1.000000000000000000, 0.000000000000000000, -0.000000000000000000 ) ) ;
#13955 = EDGE_LOOP ( 'NONE', ( #5207, #8074 ) ) ;
#13956 = ORIENTED_EDGE ( 'NONE', *, *, #9532, .F. ) ;
#13957 = EDGE_CURVE ( 'NONE', #12804, #11894, #3669, .T. ) ;
#13958 = ORIENTED_EDGE ( 'NONE', *, *, #10624, .T. ) ;
#13959 = CARTESIAN_POINT ( 'NONE',  ( 6.134011831684059501, 140.6204725398426092, 12.99999999999999822 ) ) ;
#13960 = ORIENTED_EDGE ( 'NONE', *, *, #520, .T. ) ;
#13961 = DIRECTION ( 'NONE',  ( -0.000000000000000000, -0.000000000000000000, -1.000000000000000000 ) ) ;
#13962 = VERTEX_POINT ( 'NONE', #15879 ) ;
#13963 =( NAMED_UNIT ( * ) SI_UNIT ( $, .STERADIAN. ) SOLID_ANGLE_UNIT ( ) );
#13964 = DIRECTION ( 'NONE',  ( 0.000000000000000000, 0.000000000000000000, -1.000000000000000000 ) ) ;
#13965 = DIRECTION ( 'NONE',  ( 1.000000000000000000, 0.000000000000000000, -0.000000000000000000 ) ) ;
#13966 = CARTESIAN_POINT ( 'NONE',  ( -50.00000000000000000, 171.6227766016838245, 0.000000000000000000 ) ) ;
#13967 = CARTESIAN_POINT ( 'NONE',  ( 36.41998248565997187, 142.7179894756440035, -15.94334347237690430 ) ) ;
#13968 = ORIENTED_EDGE ( 'NONE', *, *, #3935, .F. ) ;
#13969 = CARTESIAN_POINT ( 'NONE',  ( 29.51948765637180827, 141.6406938050144220, 13.78697217532817376 ) ) ;
#13970 = LINE ( 'NONE', #2817, #8754 ) ;
#13971 = CYLINDRICAL_SURFACE ( 'NONE', #16976, 5.000000000000004441 ) ;
#13972 = DIRECTION ( 'NONE',  ( 0.000000000000000000, 1.000000000000000000, 0.000000000000000000 ) ) ;
#13973 = EDGE_CURVE ( 'NONE', #544, #5825, #7554, .T. ) ;
#13974 = EDGE_CURVE ( 'NONE', #14597, #3017, #7815, .T. ) ;
#13975 = DIRECTION ( 'NONE',  ( 0.000000000000000000, 0.000000000000000000, 1.000000000000000000 ) ) ;
#13976 = ORIENTED_EDGE ( 'NONE', *, *, #1965, .F. ) ;
#13977 = PLANE ( 'NONE',  #2760 ) ;
#13978 = CIRCLE ( 'NONE', #8024, 2.375000000000000000 ) ;
#13979 = ORIENTED_EDGE ( 'NONE', *, *, #9700, .T. ) ;
#13980 =( NAMED_UNIT ( * ) PLANE_ANGLE_UNIT ( ) SI_UNIT ( $, .RADIAN. ) );
#13981 = CARTESIAN_POINT ( 'NONE',  ( 7.376038361426209278, 142.5209969267753536, 19.44444444444444642 ) ) ;
#13982 = CIRCLE ( 'NONE', #11692, 2.500000000000002220 ) ;
#13983 = ADVANCED_FACE ( 'NONE', ( #13222 ), #10213, .T. ) ;
#13984 = ORIENTED_EDGE ( 'NONE', *, *, #7281, .F. ) ;
#13985 = CARTESIAN_POINT ( 'NONE',  ( 30.00000000000000355, 196.6227766016838245, 0.000000000000000000 ) ) ;
#13986 = CARTESIAN_POINT ( 'NONE',  ( 20.21973759693270267, 29.89473369120481294, 11.02800485953945930 ) ) ;
#13987 = DIRECTION ( 'NONE',  ( 0.000000000000000000, 0.000000000000000000, 1.000000000000000000 ) ) ;
#13988 = DIRECTION ( 'NONE',  ( -0.000000000000000000, -0.000000000000000000, -1.000000000000000000 ) ) ;
#13989 = CARTESIAN_POINT ( 'NONE',  ( 22.93524650466161674, 29.84210526315774104, 5.528366322421692125 ) ) ;
#13990 = CARTESIAN_POINT ( 'NONE',  ( -78.87601194445579722, 201.4991975277559675, 14.01484360552155373 ) ) ;
#13991 = DIRECTION ( 'NONE',  ( -0.08715574274764831264, -0.4980973490458652231, -0.8627299156628261967 ) ) ;
#13992 = VECTOR ( 'NONE', #552, 1000.000000000000000 ) ;
#13993 = ORIENTED_EDGE ( 'NONE', *, *, #11334, .T. ) ;
#13994 = ORIENTED_EDGE ( 'NONE', *, *, #13239, .T. ) ;
#13995 = DIRECTION ( 'NONE',  ( -1.000000000000000000, 0.000000000000000000, 0.000000000000000000 ) ) ;
#13996 = DIRECTION ( 'NONE',  ( 0.000000000000000000, 1.000000000000000000, 0.000000000000000000 ) ) ;
#13997 = ORIENTED_EDGE ( 'NONE', *, *, #6417, .T. ) ;
#13998 = DIRECTION ( 'NONE',  ( -1.000000000000000000, 0.000000000000000000, 0.000000000000000000 ) ) ;
#13999 = CARTESIAN_POINT ( 'NONE',  ( 32.99999999999998579, 9.999999999999998224, -12.99999999999999822 ) ) ;
#14000 = EDGE_LOOP ( 'NONE', ( #14174, #8339, #12818, #4648 ) ) ;
#14001 = APPLICATION_CONTEXT ( 'automotive_design' ) ;
#14002 = CARTESIAN_POINT ( 'NONE',  ( 14.93242934743710393, 30.00000000000000000, 13.00000000000000178 ) ) ;
#14003 = EDGE_CURVE ( 'NONE', #15793, #12127, #4898, .T. ) ;
#14004 = AXIS2_PLACEMENT_3D ( 'NONE', #8778, #16925, #15329 ) ;
#14005 = CARTESIAN_POINT ( 'NONE',  ( 30.00000000000001066, 146.6227766016838245, 1.387778780781445676E-14 ) ) ;
#14006 = STYLED_ITEM ( 'NONE', ( #16477 ), #11148 ) ;
#14007 = CARTESIAN_POINT ( 'NONE',  ( -207.4350753193408536, 166.4757156568063294, -0.9174036676442806071 ) ) ;
#14008 = CARTESIAN_POINT ( 'NONE',  ( -208.0000000000000853, 170.0678595944000620, -2.693195258168412654 ) ) ;
#14009 = DIRECTION ( 'NONE',  ( -0.000000000000000000, -0.000000000000000000, -1.000000000000000000 ) ) ;
#14010 = CARTESIAN_POINT ( 'NONE',  ( -73.34636706823184227, 143.1278587772776518, -16.66575456205189454 ) ) ;
#14011 = EDGE_LOOP ( 'NONE', ( #6356, #8390, #9975, #9643 ) ) ;
#14012 = CARTESIAN_POINT ( 'NONE',  ( 25.83188736168996513, 137.9746650487458908, -9.688332914129558660 ) ) ;
#14013 = EDGE_CURVE ( 'NONE', #6313, #10830, #9266, .T. ) ;
#14014 = EDGE_LOOP ( 'NONE', ( #4363, #1137, #13365, #8676 ) ) ;
#14015 = CARTESIAN_POINT ( 'NONE',  ( 27.48361012698969930, 136.6227766016838245, 1.296296296296295614 ) ) ;
#14016 = AXIS2_PLACEMENT_3D ( 'NONE', #4318, #16270, #4407 ) ;
#14017 = FACE_BOUND ( 'NONE', #4129, .T. ) ;
#14018 = CIRCLE ( 'NONE', #10045, 7.500000000000020428 ) ;
#14019 = ORIENTED_EDGE ( 'NONE', *, *, #4139, .F. ) ;
#14020 = DIRECTION ( 'NONE',  ( -1.000000000000000000, -0.000000000000000000, -0.000000000000000000 ) ) ;
#14021 = AXIS2_PLACEMENT_3D ( 'NONE', #13242, #11644, #859 ) ;
#14022 = CIRCLE ( 'NONE', #3808, 25.00000000000000000 ) ;
#14023 = CARTESIAN_POINT ( 'NONE',  ( 17.54349574104652021, 125.4948194589026684, 5.000000000000000888 ) ) ;
#14024 = CARTESIAN_POINT ( 'NONE',  ( 23.14977753070778377, 139.1449216839932319, 13.05325656350955654 ) ) ;
#14025 = ORIENTED_EDGE ( 'NONE', *, *, #14108, .F. ) ;
#14026 = CONTEXT_DEPENDENT_SHAPE_REPRESENTATION ( #657, #5883 ) ;
#14027 = CARTESIAN_POINT ( 'NONE',  ( -50.00000000000000000, 8.000000000000000000, -40.00000000000000000 ) ) ;
#14028 = CARTESIAN_POINT ( 'NONE',  ( -100.0000000000000000, 171.6227766016838245, 0.000000000000000000 ) ) ;
#14029 = VECTOR ( 'NONE', #461, 1000.000000000000000 ) ;
#14030 = AXIS2_PLACEMENT_3D ( 'NONE', #8445, #6689, #1467 ) ;
#14031 = CARTESIAN_POINT ( 'NONE',  ( -75.92991404580537562, 193.7005638513908252, 24.52922227238014230 ) ) ;
#14032 = DIRECTION ( 'NONE',  ( 1.000000000000000000, 0.000000000000000000, 0.000000000000000000 ) ) ;
#14033 = DIRECTION ( 'NONE',  ( -1.000000000000000000, 0.000000000000000000, 0.000000000000000000 ) ) ;
#14034 = AXIS2_PLACEMENT_3D ( 'NONE', #485, #14290, #15445 ) ;
#14035 = CARTESIAN_POINT ( 'NONE',  ( -7.965954974912850872, 30.19485118722929329, -13.00000000000000178 ) ) ;
#14036 = ORIENTED_EDGE ( 'NONE', *, *, #5474, .T. ) ;
#14037 =( BOUNDED_CURVE ( )  B_SPLINE_CURVE ( 3, ( #15257, #9590, #14994, #13671 ),
 .UNSPECIFIED., .F., .F. ) 
 B_SPLINE_CURVE_WITH_KNOTS ( ( 4, 4 ),
 ( -1.776356839400250465E-15, 1.490556265852239326 ),
 .UNSPECIFIED. ) 
 CURVE ( )  GEOMETRIC_REPRESENTATION_ITEM ( )  RATIONAL_B_SPLINE_CURVE ( ( 1.000000000000000000, 0.8232662051119106206, 0.8232662051119106206, 1.000000000000000000 ) ) 
 REPRESENTATION_ITEM ( '' )  );
#14038 = CARTESIAN_POINT ( 'NONE',  ( 48.00000000000000711, 183.6227766016837961, -5.571800142134975431 ) ) ;
#14039 = ADVANCED_FACE ( 'NONE', ( #9136 ), #14543, .F. ) ;
#14040 = ADVANCED_FACE ( 'NONE', ( #7639 ), #750, .T. ) ;
#14041 = DIRECTION ( 'NONE',  ( 8.673617379884037937E-17, 0.000000000000000000, -1.000000000000000000 ) ) ;
#14042 = EDGE_CURVE ( 'NONE', #5702, #10995, #12107, .T. ) ;
#14043 = ORIENTED_EDGE ( 'NONE', *, *, #4142, .F. ) ;
#14044 = DIRECTION ( 'NONE',  ( 1.000000000000000000, 0.000000000000000000, -0.000000000000000000 ) ) ;
#14045 = CARTESIAN_POINT ( 'NONE',  ( 49.99999999999998579, 175.6227766016838245, -5.571800142134975431 ) ) ;
#14046 = ORIENTED_EDGE ( 'NONE', *, *, #15675, .T. ) ;
#14047 = ORIENTED_EDGE ( 'NONE', *, *, #5815, .T. ) ;
#14048 = ORIENTED_EDGE ( 'NONE', *, *, #14670, .T. ) ;
#14049 = VECTOR ( 'NONE', #10085, 1000.000000000000000 ) ;
#14050 = CARTESIAN_POINT ( 'NONE',  ( 9.466951579747838963, 140.2095812714875080, 12.14773935231147739 ) ) ;
#14051 = AXIS2_PLACEMENT_3D ( 'NONE', #2747, #14702, #13370 ) ;
#14052 = ORIENTED_EDGE ( 'NONE', *, *, #10792, .T. ) ;
#14053 = CARTESIAN_POINT ( 'NONE',  ( -725.0000000000000000, 19.99999999999995737, 0.000000000000000000 ) ) ;
#14054 = EDGE_LOOP ( 'NONE', ( #14527, #1774 ) ) ;
#14055 =( NAMED_UNIT ( * ) PLANE_ANGLE_UNIT ( ) SI_UNIT ( $, .RADIAN. ) );
#14056 = DIRECTION ( 'NONE',  ( -1.156482317317868274E-16, 1.000000000000000000, 0.000000000000000000 ) ) ;
#14057 =( NAMED_UNIT ( * ) PLANE_ANGLE_UNIT ( ) SI_UNIT ( $, .RADIAN. ) );
#14058 = DIRECTION ( 'NONE',  ( 0.000000000000000000, 0.000000000000000000, 1.000000000000000000 ) ) ;
#14059 = AXIS2_PLACEMENT_3D ( 'NONE', #2832, #12040, #8229 ) ;
#14060 = VERTEX_POINT ( 'NONE', #12962 ) ;
#14061 = CARTESIAN_POINT ( 'NONE',  ( 28.85491924750536796, 141.7513145237122387, 14.02541974480121034 ) ) ;
#14062 = DIRECTION ( 'NONE',  ( 1.000000000000000000, -0.000000000000000000, -0.000000000000000000 ) ) ;
#14063 = CIRCLE ( 'NONE', #6409, 9.999999999999998224 ) ;
#14064 = CARTESIAN_POINT ( 'NONE',  ( 196.0000000000000000, 167.6227766016838814, 21.92820660268601074 ) ) ;
#14065 = AXIS2_PLACEMENT_3D ( 'NONE', #15890, #9335, #6508 ) ;
#14066 = DIRECTION ( 'NONE',  ( 0.000000000000000000, 0.000000000000000000, -1.000000000000000000 ) ) ;
#14067 = PLANE ( 'NONE',  #5534 ) ;
#14068 = DIRECTION ( 'NONE',  ( -0.000000000000000000, -0.000000000000000000, -1.000000000000000000 ) ) ;
#14069 = ORIENTED_EDGE ( 'NONE', *, *, #458, .T. ) ;
#14070 = DIRECTION ( 'NONE',  ( 0.000000000000000000, -1.000000000000000000, -6.123233995736762338E-17 ) ) ;
#14071 = ORIENTED_EDGE ( 'NONE', *, *, #12549, .F. ) ;
#14072 = AXIS2_PLACEMENT_3D ( 'NONE', #9551, #6827, #2833 ) ;
#14073 = CARTESIAN_POINT ( 'NONE',  ( 17.37251483187831624, 141.0177972567464906, 16.98271123612915545 ) ) ;
#14074 = CARTESIAN_POINT ( 'NONE',  ( 49.99999999999998579, 183.6227766016837961, -3.071800142134975431 ) ) ;
#14075 = ORIENTED_EDGE ( 'NONE', *, *, #9328, .F. ) ;
#14076 = STYLED_ITEM ( 'NONE', ( #2185 ), #16934 ) ;
#14077 = LINE ( 'NONE', #3358, #6178 ) ;
#14078 = ADVANCED_FACE ( 'NONE', ( #13050 ), #838, .T. ) ;
#14079 = CARTESIAN_POINT ( 'NONE',  ( -40.00000000000000711, 0.000000000000000000, 33.00000000000000711 ) ) ;
#14080 = ORIENTED_EDGE ( 'NONE', *, *, #10468, .F. ) ;
#14081 = LINE ( 'NONE', #1851, #8114 ) ;
#14082 = FACE_OUTER_BOUND ( 'NONE', #9066, .T. ) ;
#14083 = CARTESIAN_POINT ( 'NONE',  ( -77.93947261911883118, 201.1823876344234350, 14.67159435888866525 ) ) ;
#14084 = DIRECTION ( 'NONE',  ( 1.000000000000000000, 0.000000000000000000, -0.000000000000000000 ) ) ;
#14085 = ORIENTED_EDGE ( 'NONE', *, *, #11030, .F. ) ;
#14086 = VERTEX_POINT ( 'NONE', #920 ) ;
#14087 = CARTESIAN_POINT ( 'NONE',  ( 23.71167364621568652, 19.99999999999772982, -10.06760101871518032 ) ) ;
#14088 = VECTOR ( 'NONE', #4657, 1000.000000000000000 ) ;
#14089 = CARTESIAN_POINT ( 'NONE',  ( 18.93231600135347392, 142.3609111598534298, -15.26062816855829851 ) ) ;
#14090 = ORIENTED_EDGE ( 'NONE', *, *, #496, .F. ) ;
#14091 = CARTESIAN_POINT ( 'NONE',  ( 30.00000000000000355, 196.6227766016838245, 0.000000000000000000 ) ) ;
#14092 = DIRECTION ( 'NONE',  ( 0.000000000000000000, 0.000000000000000000, 1.000000000000000000 ) ) ;
#14093 = EDGE_LOOP ( 'NONE', ( #5986, #13260, #16902, #7609 ) ) ;
#14094 = FACE_OUTER_BOUND ( 'NONE', #10032, .T. ) ;
#14095 = UNCERTAINTY_MEASURE_WITH_UNIT (LENGTH_MEASURE( 1.000000000000000082E-05 ), #11921, 'distance_accuracy_value', 'NONE');
#14096 = CARTESIAN_POINT ( 'NONE',  ( -19.25702671965663626, 18.00000000000000355, 21.36300512502526061 ) ) ;
#14097 = CIRCLE ( 'NONE', #1068, 2.375000000000000000 ) ;
#14098 = EDGE_CURVE ( 'NONE', #3793, #12895, #4824, .T. ) ;
#14099 = CARTESIAN_POINT ( 'NONE',  ( -116.4755503550297107, 171.6227766016838245, 0.000000000000000000 ) ) ;
#14100 = DIRECTION ( 'NONE',  ( 0.000000000000000000, -0.8660254037844413721, 0.4999999999999953371 ) ) ;
#14101 = CARTESIAN_POINT ( 'NONE',  ( -24.93725393319378725, 100.0000000000000142, -5.500000000000000000 ) ) ;
#14102 = CARTESIAN_POINT ( 'NONE',  ( -32.66708739526796990, 119.0939651702496178, 4.814896201975304102 ) ) ;
#14103 = CARTESIAN_POINT ( 'NONE',  ( -72.50000000000001421, 146.0561595177563845, -20.88304578468306261 ) ) ;
#14104 = VERTEX_POINT ( 'NONE', #2154 ) ;
#14105 = CARTESIAN_POINT ( 'NONE',  ( 17.37251483187831624, 141.0177972567464906, -16.98271123612915545 ) ) ;
#14106 = EDGE_CURVE ( 'NONE', #15544, #8340, #11250, .T. ) ;
#14107 = ORIENTED_EDGE ( 'NONE', *, *, #281, .F. ) ;
#14108 = EDGE_CURVE ( 'NONE', #15090, #10662, #111, .T. ) ;
#14109 = DIRECTION ( 'NONE',  ( -1.000000000000000000, 0.000000000000000000, -8.673617379884037937E-17 ) ) ;
#14110 = EDGE_CURVE ( 'NONE', #10896, #11802, #10520, .T. ) ;
#14111 = CARTESIAN_POINT ( 'NONE',  ( -27.98221281347037959, 18.00000000000000711, -5.670874406215274277 ) ) ;
#14112 = ORIENTED_EDGE ( 'NONE', *, *, #5206, .T. ) ;
#14113 = CYLINDRICAL_SURFACE ( 'NONE', #11427, 8.000000000000000000 ) ;
#14114 = CIRCLE ( 'NONE', #241, 20.00000000000000355 ) ;
#14115 = CARTESIAN_POINT ( 'NONE',  ( 24.87018239537452757, 29.86925179676151032, 6.310755877675157777 ) ) ;
#14116 = CARTESIAN_POINT ( 'NONE',  ( 26.85584576128377066, 137.3904121345421458, 7.294850950184896377 ) ) ;
#14117 = VERTEX_POINT ( 'NONE', #8075 ) ;
#14118 = DIRECTION ( 'NONE',  ( -0.000000000000000000, -0.000000000000000000, -1.000000000000000000 ) ) ;
#14119 = FACE_OUTER_BOUND ( 'NONE', #6404, .T. ) ;
#14120 = CARTESIAN_POINT ( 'NONE',  ( -79.20543317789827142, 191.6823464236538825, 26.20333082749371556 ) ) ;
#14121 = AXIS2_PLACEMENT_3D ( 'NONE', #8232, #7165, #5837 ) ;
#14122 = LINE ( 'NONE', #5881, #16159 ) ;
#14123 = CARTESIAN_POINT ( 'NONE',  ( 14.93242934743710570, 18.00000000000000000, 25.00000000000000000 ) ) ;
#14124 = AXIS2_PLACEMENT_3D ( 'NONE', #2943, #9580, #2862 ) ;
#14125 = CARTESIAN_POINT ( 'NONE',  ( -98.00000000000000000, 171.6227766016838245, -5.000000000000006217 ) ) ;
#14126 = AXIS2_PLACEMENT_3D ( 'NONE', #8555, #15460, #2010 ) ;
#14127 = ORIENTED_EDGE ( 'NONE', *, *, #10336, .F. ) ;
#14128 = CARTESIAN_POINT ( 'NONE',  ( 1.559999999999998943, 1.732050807568885631, 0.000000000000000000 ) ) ;
#14129 = CARTESIAN_POINT ( 'NONE',  ( -27.94760966554430937, 19.99999999999999645, -6.338314452217975514 ) ) ;
#14130 = VERTEX_POINT ( 'NONE', #13490 ) ;
#14131 = LINE ( 'NONE', #1998, #16387 ) ;
#14132 = CARTESIAN_POINT ( 'NONE',  ( -24.99999999999999289, 90.00000000000000000, 0.000000000000000000 ) ) ;
#14133 = EDGE_LOOP ( 'NONE', ( #14215, #3941, #12290, #17437 ) ) ;
#14134 = ORIENTED_EDGE ( 'NONE', *, *, #6721, .F. ) ;
#14135 = ORIENTED_EDGE ( 'NONE', *, *, #13389, .F. ) ;
#14136 = AXIS2_PLACEMENT_3D ( 'NONE', #7148, #6883, #413 ) ;
#14137 = VERTEX_POINT ( 'NONE', #1526 ) ;
#14138 = SURFACE_STYLE_FILL_AREA ( #3063 ) ;
#14139 = CIRCLE ( 'NONE', #1124, 5.000000000000004441 ) ;
#14140 = EDGE_LOOP ( 'NONE', ( #17002, #15235, #2024, #4536 ) ) ;
#14141 = EDGE_CURVE ( 'NONE', #10086, #4376, #14097, .T. ) ;
#14142 = ADVANCED_FACE ( 'NONE', ( #7908 ), #10824, .F. ) ;
#14143 = CARTESIAN_POINT ( 'NONE',  ( 23.34456489498957055, 143.1309386941325101, -16.67123533649925449 ) ) ;
#14144 = CARTESIAN_POINT ( 'NONE',  ( -82.50000000000001421, 196.6227766016838245, -16.00000000000000000 ) ) ;
#14145 = DIRECTION ( 'NONE',  ( -1.000000000000000000, 8.673617379884038430E-16, 0.000000000000000000 ) ) ;
#14146 = DIRECTION ( 'NONE',  ( -1.000000000000000000, -0.000000000000000000, -0.000000000000000000 ) ) ;
#14147 = ORIENTED_EDGE ( 'NONE', *, *, #2937, .T. ) ;
#14148 = DIRECTION ( 'NONE',  ( 0.000000000000000000, 0.000000000000000000, -1.000000000000000000 ) ) ;
#14149 = AXIS2_PLACEMENT_3D ( 'NONE', #4972, #15187, #13041 ) ;
#14150 = CIRCLE ( 'NONE', #13295, 5.999999999999998224 ) ;
#14151 = PLANE ( 'NONE',  #2523 ) ;
#14152 = FACE_OUTER_BOUND ( 'NONE', #1600, .T. ) ;
#14153 = VECTOR ( 'NONE', #3180, 1000.000000000000000 ) ;
#14154 = CARTESIAN_POINT ( 'NONE',  ( -12.97728802729275088, 19.99999999999999645, -11.64645903342270827 ) ) ;
#14155 = FACE_OUTER_BOUND ( 'NONE', #716, .T. ) ;
#14156 = LINE ( 'NONE', #11397, #3676 ) ;
#14157 = VERTEX_POINT ( 'NONE', #14897 ) ;
#14158 = CARTESIAN_POINT ( 'NONE',  ( 37.99999999999998579, 2.000000000000000000, 28.00000000000001066 ) ) ;
#14159 = VECTOR ( 'NONE', #3689, 1000.000000000000000 ) ;
#14160 = ORIENTED_EDGE ( 'NONE', *, *, #12799, .T. ) ;
#14161 = ADVANCED_FACE ( 'NONE', ( #202 ), #15960, .F. ) ;
#14162 = EDGE_CURVE ( 'NONE', #3065, #16797, #16653, .T. ) ;
#14163 = CARTESIAN_POINT ( 'NONE',  ( -74.00000000000001421, 196.6227766016838245, -35.00000000000000000 ) ) ;
#14164 = ADVANCED_FACE ( 'NONE', ( #15248 ), #5613, .T. ) ;
#14165 = AXIS2_PLACEMENT_3D ( 'NONE', #6967, #5644, #16455 ) ;
#14166 = ADVANCED_FACE ( 'NONE', ( #7372, #13847, #8430 ), #555, .F. ) ;
#14167 = LINE ( 'NONE', #9004, #7861 ) ;
#14168 = CARTESIAN_POINT ( 'NONE',  ( 15.56337975240373872, 125.2134999403456135, -4.999999999999997335 ) ) ;
#14169 = EDGE_LOOP ( 'NONE', ( #9062, #5297, #15873, #3901 ) ) ;
#14170 = DIRECTION ( 'NONE',  ( 1.000000000000000000, 0.000000000000000000, -8.673617379884037937E-17 ) ) ;
#14171 = DIRECTION ( 'NONE',  ( 1.000000000000000000, 0.000000000000000000, 0.000000000000000000 ) ) ;
#14172 = CARTESIAN_POINT ( 'NONE',  ( -85.00000000000001421, 197.2415780845126676, 20.82248078717324091 ) ) ;
#14173 = CARTESIAN_POINT ( 'NONE',  ( 26.85383255238284761, 201.7487681645689861, -17.82060658420952493 ) ) ;
#14174 = ORIENTED_EDGE ( 'NONE', *, *, #8799, .F. ) ;
#14175 = CIRCLE ( 'NONE', #15005, 19.01029467089431080 ) ;
#14176 = ORIENTED_EDGE ( 'NONE', *, *, #12456, .F. ) ;
#14177 = CARTESIAN_POINT ( 'NONE',  ( 19.93228116232496205, 29.93335004877557282, -13.66730128329526650 ) ) ;
#14178 = CARTESIAN_POINT ( 'NONE',  ( 26.51307711398865408, 139.5431919169737967, -7.747420853565629706 ) ) ;
#14179 = ORIENTED_EDGE ( 'NONE', *, *, #155, .T. ) ;
#14180 = EDGE_CURVE ( 'NONE', #11846, #9474, #3067, .T. ) ;
#14181 = FACE_OUTER_BOUND ( 'NONE', #5800, .T. ) ;
#14182 = DIRECTION ( 'NONE',  ( 0.000000000000000000, 1.000000000000000000, 0.000000000000000000 ) ) ;
#14183 = ORIENTED_EDGE ( 'NONE', *, *, #700, .F. ) ;
#14184 = LINE ( 'NONE', #1957, #9596 ) ;
#14185 = CIRCLE ( 'NONE', #14748, 33.00000000000000000 ) ;
#14186 = CARTESIAN_POINT ( 'NONE',  ( -207.2467692809710229, 166.5426260787756974, -0.7960839355505516801 ) ) ;
#14187 = PLANE ( 'NONE',  #15120 ) ;
#14188 = CARTESIAN_POINT ( 'NONE',  ( -14.55266450408069723, 18.00000000000000000, 23.76398220081675206 ) ) ;
#14189 = CARTESIAN_POINT ( 'NONE',  ( -31.89848094669886436, 119.9728602285818084, 5.500000000000000000 ) ) ;
#14190 = LINE ( 'NONE', #1071, #13434 ) ;
#14191 = ORIENTED_EDGE ( 'NONE', *, *, #9479, .F. ) ;
#14192 = CARTESIAN_POINT ( 'NONE',  ( -77.50000000000002842, 146.6227766016838245, 0.000000000000000000 ) ) ;
#14193 = ORIENTED_EDGE ( 'NONE', *, *, #935, .T. ) ;
#14194 = CARTESIAN_POINT ( 'NONE',  ( 34.99999999999999289, -20.00000000000000000, 34.99999999999999289 ) ) ;
#14195 = FACE_OUTER_BOUND ( 'NONE', #16527, .T. ) ;
#14196 = ORIENTED_EDGE ( 'NONE', *, *, #884, .F. ) ;
#14197 = EDGE_CURVE ( 'NONE', #16730, #1036, #2501, .T. ) ;
#14198 = DIRECTION ( 'NONE',  ( -0.000000000000000000, -0.000000000000000000, -1.000000000000000000 ) ) ;
#14199 = CARTESIAN_POINT ( 'NONE',  ( 24.93507336697353338, 29.86842105263157521, 5.000000000000004441 ) ) ;
#14200 = CARTESIAN_POINT ( 'NONE',  ( 13.66217116581496249, 130.1207327347060527, 12.31521373833130717 ) ) ;
#14201 = EDGE_LOOP ( 'NONE', ( #10038, #2153, #4410, #9811 ) ) ;
#14202 = ADVANCED_FACE ( 'NONE', ( #3124, #2941, #12682 ), #9932, .F. ) ;
#14203 = FACE_OUTER_BOUND ( 'NONE', #3888, .T. ) ;
#14204 = EDGE_CURVE ( 'NONE', #15970, #14594, #11162, .T. ) ;
#14205 = CARTESIAN_POINT ( 'NONE',  ( -82.56615862916986259, 192.3153571870206804, 25.70724251753716061 ) ) ;
#14206 = CARTESIAN_POINT ( 'NONE',  ( -50.00000000000000000, 171.6227766016838245, 0.000000000000000000 ) ) ;
#14207 = CARTESIAN_POINT ( 'NONE',  ( -3.000000000000002665, 144.1839557653416080, -18.33333333333336057 ) ) ;
#14208 = LINE ( 'NONE', #11538, #6325 ) ;
#14209 = ORIENTED_EDGE ( 'NONE', *, *, #3030, .T. ) ;
#14210 = DIRECTION ( 'NONE',  ( -0.000000000000000000, -0.000000000000000000, 1.000000000000000000 ) ) ;
#14211 = LINE ( 'NONE', #664, #3700 ) ;
#14212 = ORIENTED_EDGE ( 'NONE', *, *, #13749, .T. ) ;
#14213 = CYLINDRICAL_SURFACE ( 'NONE', #1393, 2.000000000000001776 ) ;
#14214 = DIRECTION ( 'NONE',  ( -1.156482317317868274E-16, 1.000000000000000000, 0.000000000000000000 ) ) ;
#14215 = ORIENTED_EDGE ( 'NONE', *, *, #11617, .F. ) ;
#14216 = ORIENTED_EDGE ( 'NONE', *, *, #1922, .T. ) ;
#14217 = EDGE_LOOP ( 'NONE', ( #14179, #2785, #6791, #2629 ) ) ;
#14218 = VERTEX_POINT ( 'NONE', #10006 ) ;
#14219 = CARTESIAN_POINT ( 'NONE',  ( -20.00000000000000355, 171.6227766016838245, 19.49999999999998934 ) ) ;
#14220 = ORIENTED_EDGE ( 'NONE', *, *, #8285, .T. ) ;
#14221 = CARTESIAN_POINT ( 'NONE',  ( 22.50000000000001421, 146.0571958828608672, -20.88424858573642595 ) ) ;
#14222 = DIRECTION ( 'NONE',  ( 0.000000000000000000, 0.000000000000000000, 1.000000000000000000 ) ) ;
#14223 = EDGE_CURVE ( 'NONE', #9474, #11846, #17201, .T. ) ;
#14224 = CARTESIAN_POINT ( 'NONE',  ( -80.00000000000002842, 146.6227766016838245, 35.00200000000000244 ) ) ;
#14225 = CARTESIAN_POINT ( 'NONE',  ( 27.48361012698968864, 138.6227766016838245, 1.063447695028167043E-14 ) ) ;
#14226 = ORIENTED_EDGE ( 'NONE', *, *, #13390, .F. ) ;
#14227 = CARTESIAN_POINT ( 'NONE',  ( 28.45845633961465992, 141.8618947663538279, 14.25856086977510984 ) ) ;
#14228 = CARTESIAN_POINT ( 'NONE',  ( -70.00000000000000000, 154.3022685259950038, 9.999999999999900524 ) ) ;
#14229 = DIRECTION ( 'NONE',  ( 0.000000000000000000, 1.000000000000000000, -1.224646799147353207E-16 ) ) ;
#14230 = CARTESIAN_POINT ( 'NONE',  ( -10.87333020471588974, 20.00000000000114753, -13.51515657978521645 ) ) ;
#14231 = PRESENTATION_STYLE_ASSIGNMENT (( #3350 ) ) ;
#14232 = EDGE_CURVE ( 'NONE', #4814, #4046, #5046, .T. ) ;
#14233 = B_SPLINE_CURVE_WITH_KNOTS ( 'NONE', 3,
 ( #15059, #13486, #14894, #13580 ),
 .UNSPECIFIED., .F., .F.,
 ( 4, 4 ),
 ( 0.000000000000000000, 0.003672568685860802366 ),
 .UNSPECIFIED. ) ;
#14234 = DIRECTION ( 'NONE',  ( -1.000000000000000000, -0.000000000000000000, 0.000000000000000000 ) ) ;
#14235 = ORIENTED_EDGE ( 'NONE', *, *, #3971, .F. ) ;
#14236 = PLANE ( 'NONE',  #11508 ) ;
#14237 = ORIENTED_EDGE ( 'NONE', *, *, #2959, .T. ) ;
#14238 = CARTESIAN_POINT ( 'NONE',  ( -31.66708739526795924, 120.0000000000000284, 5.500000000000000000 ) ) ;
#14239 = DIRECTION ( 'NONE',  ( 1.000000000000000000, 0.000000000000000000, 0.000000000000000000 ) ) ;
#14240 = CARTESIAN_POINT ( 'NONE',  ( -153.0000000000000284, 171.6227766016838245, 23.57392898041431195 ) ) ;
#14241 = ORIENTED_EDGE ( 'NONE', *, *, #8003, .F. ) ;
#14242 = DIRECTION ( 'NONE',  ( -0.000000000000000000, -0.000000000000000000, -1.000000000000000000 ) ) ;
#14243 = CARTESIAN_POINT ( 'NONE',  ( -80.00000000000002842, 146.6227766016838245, -35.00000000000000000 ) ) ;
#14244 = DIRECTION ( 'NONE',  ( -1.000000000000000000, 0.000000000000000000, 0.000000000000000000 ) ) ;
#14245 = CARTESIAN_POINT ( 'NONE',  ( 31.43242313191838022, 202.4505251070389420, -16.57269434321683477 ) ) ;
#14246 = ORIENTED_EDGE ( 'NONE', *, *, #17287, .T. ) ;
#14247 = ADVANCED_FACE ( 'NONE', ( #11352 ), #14378, .T. ) ;
#14248 = EDGE_CURVE ( 'NONE', #15075, #10212, #4767, .T. ) ;
#14249 = EDGE_CURVE ( 'NONE', #9334, #3454, #3782, .T. ) ;
#14250 = VERTEX_POINT ( 'NONE', #17015 ) ;
#14251 = CARTESIAN_POINT ( 'NONE',  ( 25.49876332522151401, 19.99999999999999645, -21.99427390110736624 ) ) ;
#14252 = DIRECTION ( 'NONE',  ( 0.000000000000000000, 0.000000000000000000, -1.000000000000000000 ) ) ;
#14253 = VERTEX_POINT ( 'NONE', #3734 ) ;
#14254 = CARTESIAN_POINT ( 'NONE',  ( -100.0000000000000000, 134.2062027339443944, 25.00000000000000000 ) ) ;
#14255 = CARTESIAN_POINT ( 'NONE',  ( 6.134011831684059501, 134.2062027339443944, -13.00000000000000000 ) ) ;
#14256 = VERTEX_POINT ( 'NONE', #6377 ) ;
#14257 = DIRECTION ( 'NONE',  ( 0.9961946980917465444, -0.04357787137382451714, 0.07547908730516460218 ) ) ;
#14258 = FACE_OUTER_BOUND ( 'NONE', #13100, .T. ) ;
#14259 = VECTOR ( 'NONE', #2685, 1000.000000000000000 ) ;
#14260 = DIRECTION ( 'NONE',  ( -1.000000000000000000, -0.000000000000000000, -0.000000000000000000 ) ) ;
#14261 = CARTESIAN_POINT ( 'NONE',  ( -26.11264420168958722, 18.00000000000000000, 13.35921939055965524 ) ) ;
#14262 = VECTOR ( 'NONE', #6705, 1000.000000000000000 ) ;
#14263 = LINE ( 'NONE', #2130, #14272 ) ;
#14264 = DIRECTION ( 'NONE',  ( 0.000000000000000000, 0.000000000000000000, -1.000000000000000000 ) ) ;
#14265 = ORIENTED_EDGE ( 'NONE', *, *, #12630, .T. ) ;
#14266 = DIRECTION ( 'NONE',  ( -1.000000000000000000, -0.000000000000000000, 0.000000000000000000 ) ) ;
#14267 = ORIENTED_EDGE ( 'NONE', *, *, #9705, .T. ) ;
#14268 = FACE_OUTER_BOUND ( 'NONE', #13039, .T. ) ;
#14269 = DIRECTION ( 'NONE',  ( 0.000000000000000000, 0.000000000000000000, 1.000000000000000000 ) ) ;
#14270 = VERTEX_POINT ( 'NONE', #10195 ) ;
#14271 = CARTESIAN_POINT ( 'NONE',  ( -15.00000000000001421, 20.00000000000004263, 4.999999999999999112 ) ) ;
#14272 = VECTOR ( 'NONE', #10449, 1000.000000000000000 ) ;
#14273 = AXIS2_PLACEMENT_3D ( 'NONE', #2133, #15768, #2311 ) ;
#14274 = CARTESIAN_POINT ( 'NONE',  ( 19.08196460475218714, 19.99999999999773337, 14.16502029867040235 ) ) ;
#14275 = ORIENTED_EDGE ( 'NONE', *, *, #5544, .F. ) ;
#14276 = FACE_OUTER_BOUND ( 'NONE', #3376, .T. ) ;
#14277 = CARTESIAN_POINT ( 'NONE',  ( -79.01193031122193133, 191.7175861903016312, 26.17636150746912094 ) ) ;
#14278 = LINE ( 'NONE', #11696, #13042 ) ;
#14279 = PLANE ( 'NONE',  #487 ) ;
#14280 = CARTESIAN_POINT ( 'NONE',  ( -100.0000000000000000, 171.6227766016838245, 0.000000000000000000 ) ) ;
#14281 = ADVANCED_FACE ( 'NONE', ( #7446 ), #10103, .T. ) ;
#14282 = AXIS2_PLACEMENT_3D ( 'NONE', #724, #6117, #972 ) ;
#14283 = ORIENTED_EDGE ( 'NONE', *, *, #17229, .F. ) ;
#14284 = CARTESIAN_POINT ( 'NONE',  ( -208.0000000000000853, 216.6520346255402956, -29.58858125237329162 ) ) ;
#14286 = CARTESIAN_POINT ( 'NONE',  ( -85.00000000000002842, 196.6227766016838245, 0.000000000000000000 ) ) ;
#14285 = AXIS2_PLACEMENT_3D ( 'NONE', #6651, #1243, #16133 ) ;
#14287 = VERTEX_POINT ( 'NONE', #15509 ) ;
#14288 = CARTESIAN_POINT ( 'NONE',  ( 32.21490539657202845, 191.0296277843086727, -29.12775510238319399 ) ) ;
#14289 = VECTOR ( 'NONE', #15228, 1000.000000000000000 ) ;
#14290 = DIRECTION ( 'NONE',  ( 1.000000000000000000, 0.000000000000000000, 0.000000000000000000 ) ) ;
#14291 = AXIS2_PLACEMENT_3D ( 'NONE', #14859, #16380, #16466 ) ;
#14292 = EDGE_LOOP ( 'NONE', ( #13882, #4072, #12398, #3750 ) ) ;
#14293 = EDGE_LOOP ( 'NONE', ( #1247, #11172, #9601, #1098 ) ) ;
#14294 = EDGE_LOOP ( 'NONE', ( #7377, #6878, #6360, #1093 ) ) ;
#14295 = CARTESIAN_POINT ( 'NONE',  ( 39.99999999999998579, 4.000000000000007105, 30.00000000000001421 ) ) ;
#14296 = VERTEX_POINT ( 'NONE', #11610 ) ;
#14297 = CARTESIAN_POINT ( 'NONE',  ( -13.22984127103138796, 31.85746429949665881, 11.06592603413638898 ) ) ;
#14298 = CIRCLE ( 'NONE', #16279, 149.9999999999999716 ) ;
#14299 = CARTESIAN_POINT ( 'NONE',  ( -24.94987437106621542, 20.00000000000004263, -5.999999999999992895 ) ) ;
#14300 = CARTESIAN_POINT ( 'NONE',  ( 48.00000000000000711, 163.6227766016838530, 15.00000337241049486 ) ) ;
#14301 = DIRECTION ( 'NONE',  ( 0.000000000000000000, -0.8660254037844413721, -0.4999999999999953371 ) ) ;
#14302 = CARTESIAN_POINT ( 'NONE',  ( -45.00000000000000000, 136.6227766016838245, 0.000000000000000000 ) ) ;
#14303 = ADVANCED_FACE ( 'NONE', ( #4963 ), #15595, .F. ) ;
#14304 = EDGE_LOOP ( 'NONE', ( #3607, #11029 ) ) ;
#14305 = DIRECTION ( 'NONE',  ( 8.673617379884037937E-17, 0.000000000000000000, -1.000000000000000000 ) ) ;
#14306 = DIRECTION ( 'NONE',  ( 0.000000000000000000, 0.9938079899999066047, 0.1111111111111111188 ) ) ;
#14307 = FACE_OUTER_BOUND ( 'NONE', #14201, .T. ) ;
#14308 = PLANE ( 'NONE',  #4214 ) ;
#14309 = AXIS2_PLACEMENT_3D ( 'NONE', #830, #11971, #13215 ) ;
#14310 = EDGE_CURVE ( 'NONE', #10464, #13669, #2223, .T. ) ;
#14311 = VECTOR ( 'NONE', #12447, 1000.000000000000000 ) ;
#14312 = EDGE_CURVE ( 'NONE', #16894, #14086, #4881, .T. ) ;
#14313 = ADVANCED_FACE ( 'NONE', ( #17092 ), #10358, .T. ) ;
#14314 = DIRECTION ( 'NONE',  ( -0.000000000000000000, -0.000000000000000000, 1.000000000000000000 ) ) ;
#14315 = ORIENTED_EDGE ( 'NONE', *, *, #6887, .F. ) ;
#14316 = CARTESIAN_POINT ( 'NONE',  ( 2.370000000000000551, 0.000000000000000000, 0.000000000000000000 ) ) ;
#14317 = DIRECTION ( 'NONE',  ( 1.000000000000000000, 0.000000000000000000, 0.000000000000000000 ) ) ;
#14318 = ORIENTED_EDGE ( 'NONE', *, *, #16898, .F. ) ;
#14319 = LINE ( 'NONE', #10067, #10742 ) ;
#14320 = AXIS2_PLACEMENT_3D ( 'NONE', #980, #16140, #14718 ) ;
#14321 = AXIS2_PLACEMENT_3D ( 'NONE', #6466, #14440, #9115 ) ;
#14322 = CARTESIAN_POINT ( 'NONE',  ( -23.00000000000000000, 122.0000000000000284, 0.000000000000000000 ) ) ;
#14323 = ADVANCED_FACE ( 'NONE', ( #9120 ), #7788, .F. ) ;
#14324 = DIRECTION ( 'NONE',  ( -1.000000000000000000, -0.000000000000000000, -0.000000000000000000 ) ) ;
#14325 = AXIS2_PLACEMENT_3D ( 'NONE', #15642, #3517, #9976 ) ;
#14326 = ORIENTED_EDGE ( 'NONE', *, *, #12254, .F. ) ;
#14327 = CARTESIAN_POINT ( 'NONE',  ( -48.00000000000000000, 204.6227766016838245, 0.000000000000000000 ) ) ;
#14328 = CARTESIAN_POINT ( 'NONE',  ( -5.000000000000004441, 134.2062027339443944, 25.00000000000000000 ) ) ;
#14329 = APPLICATION_CONTEXT ( 'automotive_design' ) ;
#14330 = CARTESIAN_POINT ( 'NONE',  ( 50.00000000000000000, 171.6227766016838245, 0.000000000000000000 ) ) ;
#14331 = PRESENTATION_STYLE_ASSIGNMENT (( #5032 ) ) ;
#14332 = VERTEX_POINT ( 'NONE', #15673 ) ;
#14333 = ORIENTED_EDGE ( 'NONE', *, *, #16098, .F. ) ;
#14334 = CARTESIAN_POINT ( 'NONE',  ( 21.03709756577793399, 29.91885446100015145, -12.94894061605241831 ) ) ;
#14335 = FACE_OUTER_BOUND ( 'NONE', #9521, .T. ) ;
#14336 = AXIS2_PLACEMENT_3D ( 'NONE', #8304, #6898, #12296 ) ;
#14337 = ORIENTED_EDGE ( 'NONE', *, *, #15468, .T. ) ;
#14338 = COLOUR_RGB ( '', 0.66274510, 0.83137255, 0.94901961) ;
#14339 = CARTESIAN_POINT ( 'NONE',  ( 196.0000000000000000, 155.6227766016839098, 12.50000337241049309 ) ) ;
#14340 = AXIS2_PLACEMENT_3D ( 'NONE', #8019, #5550, #4228 ) ;
#14341 = DIRECTION ( 'NONE',  ( -1.000000000000000000, 0.000000000000000000, 1.541976423090495387E-16 ) ) ;
#14342 = VERTEX_POINT ( 'NONE', #11520 ) ;
#14343 = CARTESIAN_POINT ( 'NONE',  ( 35.89213624354478327, 201.2861607625691818, -14.48320912595415422 ) ) ;
#14344 = B_SPLINE_CURVE_WITH_KNOTS ( 'NONE', 3,
 ( #2684, #1358, #5244, #1448 ),
 .UNSPECIFIED., .F., .F.,
 ( 4, 4 ),
 ( 0.004999999999999983624, 0.009999999999999993269 ),
 .UNSPECIFIED. ) ;
#14345 = EDGE_CURVE ( 'NONE', #12401, #9730, #729, .T. ) ;
#14346 = ADVANCED_FACE ( 'NONE', ( #904 ), #9036, .T. ) ;
#14347 = ADVANCED_FACE ( 'NONE', ( #8945 ), #14357, .T. ) ;
#14348 = DIRECTION ( 'NONE',  ( -0.000000000000000000, -0.000000000000000000, -1.000000000000000000 ) ) ;
#14349 = CARTESIAN_POINT ( 'NONE',  ( 48.00000000000000711, 167.6227766016838814, 19.42820660268601074 ) ) ;
#14350 = CARTESIAN_POINT ( 'NONE',  ( -11.84409501751983207, 17.99999999999999645, 9.388895791866135099 ) ) ;
#14351 = AXIS2_PLACEMENT_3D ( 'NONE', #2561, #9182, #11928 ) ;
#14352 = CARTESIAN_POINT ( 'NONE',  ( -45.00000000000000000, 130.0000000000000000, -15.00000000000000000 ) ) ;
#14353 = AXIS2_PLACEMENT_3D ( 'NONE', #10485, #3761, #9149 ) ;
#14354 = AXIS2_PLACEMENT_3D ( 'NONE', #3802, #8045, #14862 ) ;
#14355 = CARTESIAN_POINT ( 'NONE',  ( 31.05826940171251138, 140.7111270992951404, -16.41570701070894245 ) ) ;
#14356 = ORIENTED_EDGE ( 'NONE', *, *, #1727, .T. ) ;
#14357 = PLANE ( 'NONE',  #1943 ) ;
#14358 = ORIENTED_EDGE ( 'NONE', *, *, #6625, .F. ) ;
#14359 = DIRECTION ( 'NONE',  ( 2.312964634635742464E-16, 0.000000000000000000, -1.000000000000000000 ) ) ;
#14360 = CARTESIAN_POINT ( 'NONE',  ( -27.29618490519992591, 18.00000000000000000, -10.29570512375934044 ) ) ;
#14361 = ORIENTED_EDGE ( 'NONE', *, *, #8406, .F. ) ;
#14362 = CARTESIAN_POINT ( 'NONE',  ( 17.55923266082603007, 19.99999999999999645, 24.87049340120105612 ) ) ;
#14363 = CARTESIAN_POINT ( 'NONE',  ( 12.23870813552851722, 139.5070109101417302, 10.31054875319067143 ) ) ;
#14364 = AXIS2_PLACEMENT_3D ( 'NONE', #5269, #15083, #10764 ) ;
#14365 = CARTESIAN_POINT ( 'NONE',  ( 32.90650748920315039, 19.99999999999999645, 13.87185692902932921 ) ) ;
#14366 = AXIS2_PLACEMENT_3D ( 'NONE', #4512, #260, #9814 ) ;
#14367 =( GEOMETRIC_REPRESENTATION_CONTEXT ( 3 ) GLOBAL_UNCERTAINTY_ASSIGNED_CONTEXT ( ( #3789 ) ) GLOBAL_UNIT_ASSIGNED_CONTEXT ( ( #696, #13980, #2099 ) ) REPRESENTATION_CONTEXT ( 'NONE', 'WORKASPACE' ) );
#14368 = ORIENTED_EDGE ( 'NONE', *, *, #4441, .T. ) ;
#14369 = EDGE_CURVE ( 'NONE', #6576, #3421, #13110, .T. ) ;
#14370 = EDGE_CURVE ( 'NONE', #14513, #12401, #9278, .T. ) ;
#14371 = EDGE_CURVE ( 'NONE', #14379, #4320, #11682, .T. ) ;
#14372 = DIRECTION ( 'NONE',  ( 0.000000000000000000, 0.000000000000000000, 1.000000000000000000 ) ) ;
#14373 = CARTESIAN_POINT ( 'NONE',  ( 33.78675088369337942, 190.1432158455537262, -27.31345131271290327 ) ) ;
#14374 = DIRECTION ( 'NONE',  ( -1.000000000000000000, 0.000000000000000000, 0.000000000000000000 ) ) ;
#14375 = CARTESIAN_POINT ( 'NONE',  ( -27.84784281930893357, 18.00000000000000000, -7.647248539284095870 ) ) ;
#14376 = ORIENTED_EDGE ( 'NONE', *, *, #15204, .F. ) ;
#14377 = CARTESIAN_POINT ( 'NONE',  ( 48.00000000000000711, 151.6227766016839098, 5.571800142134973655 ) ) ;
#14378 = TOROIDAL_SURFACE ( 'NONE', #12963, -126.3651973469810628, 149.9999999999999716 ) ;
#14379 = VERTEX_POINT ( 'NONE', #10452 ) ;
#14380 = CARTESIAN_POINT ( 'NONE',  ( 24.00000000000001066, 196.3062978594714707, -24.81790219152271604 ) ) ;
#14381 = AXIS2_PLACEMENT_3D ( 'NONE', #242, #9793, #13795 ) ;
#14382 = CARTESIAN_POINT ( 'NONE',  ( -45.00000000000000000, 140.0000000000000000, -15.00000000000000000 ) ) ;
#14383 = ADVANCED_BREP_SHAPE_REPRESENTATION ( '', ( #11148, #3583 ), #4757 ) ;
#14384 = VERTEX_POINT ( 'NONE', #15860 ) ;
#14385 = ORIENTED_EDGE ( 'NONE', *, *, #16931, .F. ) ;
#14386 = ORIENTED_EDGE ( 'NONE', *, *, #7843, .T. ) ;
#14387 = ADVANCED_FACE ( 'NONE', ( #643 ), #6040, .F. ) ;
#14388 = CARTESIAN_POINT ( 'NONE',  ( -82.26120111208031460, 153.7971187266995514, -27.77174765869275674 ) ) ;
#14389 = AXIS2_PLACEMENT_3D ( 'NONE', #11407, #3363, #2032 ) ;
#14390 = ORIENTED_EDGE ( 'NONE', *, *, #9045, .F. ) ;
#14391 = CARTESIAN_POINT ( 'NONE',  ( 0.000000000000000000, 0.000000000000000000, 0.000000000000000000 ) ) ;
#14392 = CIRCLE ( 'NONE', #6480, 2.500000000000002220 ) ;
#14393 = CARTESIAN_POINT ( 'NONE',  ( -31.66708739526795924, 101.0000000000000142, -5.500000000000000000 ) ) ;
#14394 = CARTESIAN_POINT ( 'NONE',  ( -14.33532356861720380, 31.51408589783374126, 12.70909354450696149 ) ) ;
#14395 = DIRECTION ( 'NONE',  ( -0.000000000000000000, -0.000000000000000000, -1.000000000000000000 ) ) ;
#14396 = CARTESIAN_POINT ( 'NONE',  ( 23.09107716925733911, 17.99999999999999645, 5.000000000000003553 ) ) ;
#14397 = CARTESIAN_POINT ( 'NONE',  ( 27.47046887122067105, 138.6908793960143669, 2.448156880351273657 ) ) ;
#14398 = ORIENTED_EDGE ( 'NONE', *, *, #8565, .F. ) ;
#14399 = CARTESIAN_POINT ( 'NONE',  ( 16.87754908408646415, 142.8876428028120813, 16.22928829806427942 ) ) ;
#14400 = LINE ( 'NONE', #11307, #16677 ) ;
#14401 = DIRECTION ( 'NONE',  ( -1.156482317317868274E-16, 1.000000000000000000, 0.000000000000000000 ) ) ;
#14402 = CARTESIAN_POINT ( 'NONE',  ( 24.29886777166023393, 29.87658293154515832, 8.524716167024733338 ) ) ;
#14403 = ORIENTED_EDGE ( 'NONE', *, *, #12167, .T. ) ;
#14404 = CARTESIAN_POINT ( 'NONE',  ( -80.00000000000001421, 196.6227766016838245, -13.00000000000000000 ) ) ;
#14405 = VECTOR ( 'NONE', #9366, 1000.000000000000000 ) ;
#14406 = CIRCLE ( 'NONE', #16111, 4.999999999999997335 ) ;
#14407 = CIRCLE ( 'NONE', #12992, 20.00000000000000355 ) ;
#14408 = CARTESIAN_POINT ( 'NONE',  ( -187.6513770290095238, 172.4976050944027008, 4.898587196589412829E-16 ) ) ;
#14409 = ORIENTED_EDGE ( 'NONE', *, *, #5922, .T. ) ;
#14410 = EDGE_CURVE ( 'NONE', #3475, #10732, #16135, .T. ) ;
#14411 = PLANE ( 'NONE',  #12930 ) ;
#14412 = DIRECTION ( 'NONE',  ( -0.000000000000000000, -0.000000000000000000, -1.000000000000000000 ) ) ;
#14413 = ORIENTED_EDGE ( 'NONE', *, *, #10509, .T. ) ;
#14414 = CARTESIAN_POINT ( 'NONE',  ( -77.32048138630932499, 142.3872899932706559, 15.31067380954019796 ) ) ;
#14415 = PLANE ( 'NONE',  #3827 ) ;
#14416 = DIRECTION ( 'NONE',  ( -1.000000000000000000, -0.000000000000000000, -0.000000000000000000 ) ) ;
#14417 = AXIS2_PLACEMENT_3D ( 'NONE', #4862, #883, #14244 ) ;
#14418 = EDGE_CURVE ( 'NONE', #7915, #1561, #8996, .T. ) ;
#14419 = VECTOR ( 'NONE', #523, 1000.000000000000000 ) ;
#14420 = LINE ( 'NONE', #4775, #1534 ) ;
#14421 = EDGE_CURVE ( 'NONE', #4566, #6914, #14794, .T. ) ;
#14422 = ORIENTED_EDGE ( 'NONE', *, *, #12303, .T. ) ;
#14423 = DIRECTION ( 'NONE',  ( -0.000000000000000000, -0.000000000000000000, 1.000000000000000000 ) ) ;
#14424 = CARTESIAN_POINT ( 'NONE',  ( 49.99999999999998579, 191.6227766016837677, 5.571800142134975431 ) ) ;
#14425 = DIRECTION ( 'NONE',  ( -1.000000000000000000, 0.000000000000000000, 0.000000000000000000 ) ) ;
#14426 = CARTESIAN_POINT ( 'NONE',  ( 25.68011308532417303, 200.8020376890377179, -19.33395870482234713 ) ) ;
#14427 = ORIENTED_EDGE ( 'NONE', *, *, #3215, .T. ) ;
#14428 = ORIENTED_EDGE ( 'NONE', *, *, #15036, .T. ) ;
#14429 = CARTESIAN_POINT ( 'NONE',  ( 18.15033819753324806, 29.95689775512239805, -14.47405640211066213 ) ) ;
#14430 = CIRCLE ( 'NONE', #17242, 5.000000000000018652 ) ;
#14431 = CIRCLE ( 'NONE', #2570, 2.500000000000002220 ) ;
#14432 = DIRECTION ( 'NONE',  ( 0.000000000000000000, -0.000000000000000000, -1.000000000000000000 ) ) ;
#14433 = VERTEX_POINT ( 'NONE', #10627 ) ;
#14434 = CARTESIAN_POINT ( 'NONE',  ( -77.20768774440396953, 151.9379092097359489, -28.93992015514736238 ) ) ;
#14435 = AXIS2_PLACEMENT_3D ( 'NONE', #16792, #15546, #3424 ) ;
#14436 = CARTESIAN_POINT ( 'NONE',  ( 14.80221254542069076, 126.7206120434983490, -7.900896541359456293 ) ) ;
#14437 = ORIENTED_EDGE ( 'NONE', *, *, #13556, .T. ) ;
#14438 = CARTESIAN_POINT ( 'NONE',  ( 17.00000000000000000, 154.3022685259950038, 9.999999999999900524 ) ) ;
#14439 = LINE ( 'NONE', #12783, #230 ) ;
#14440 = DIRECTION ( 'NONE',  ( 0.000000000000000000, 0.000000000000000000, 1.000000000000000000 ) ) ;
#14441 = FACE_OUTER_BOUND ( 'NONE', #3282, .T. ) ;
#14442 = AXIS2_PLACEMENT_3D ( 'NONE', #16443, #4305, #8360 ) ;
#14443 = CARTESIAN_POINT ( 'NONE',  ( -26.90043998675938397, 18.00000000000000000, 11.53672424425030840 ) ) ;
#14444 = CARTESIAN_POINT ( 'NONE',  ( -45.00000000000001421, 124.1421356237309368, -15.00000000000000355 ) ) ;
#14445 = DIRECTION ( 'NONE',  ( -0.8660254037844378194, -0.5000000000000015543, -0.000000000000000000 ) ) ;
#14446 = VERTEX_POINT ( 'NONE', #13378 ) ;
#14447 = CARTESIAN_POINT ( 'NONE',  ( 7.376038361426209278, 142.5209969267753536, -19.44444444444444642 ) ) ;
#14448 = ORIENTED_EDGE ( 'NONE', *, *, #12304, .F. ) ;
#14449 = CYLINDRICAL_SURFACE ( 'NONE', #14632, 7.500000000000020428 ) ;
#14450 = CARTESIAN_POINT ( 'NONE',  ( -17.58288004918493996, 18.00000000000000000, -22.43027208364173575 ) ) ;
#14451 = EDGE_CURVE ( 'NONE', #7474, #1173, #2091, .T. ) ;
#14452 = ORIENTED_EDGE ( 'NONE', *, *, #3388, .F. ) ;
#14453 = CARTESIAN_POINT ( 'NONE',  ( -9.703671380219899945, 20.00000000000115463, 14.18606485937966788 ) ) ;
#14454 = CARTESIAN_POINT ( 'NONE',  ( 7.010070850708371992, 140.5745599005093425, 12.93128425349117983 ) ) ;
#14455 = CARTESIAN_POINT ( 'NONE',  ( 24.40970717605596718, 29.87515913883691354, 8.215055496182330330 ) ) ;
#14456 = ORIENTED_EDGE ( 'NONE', *, *, #6876, .F. ) ;
#14457 = PLANE ( 'NONE',  #3566 ) ;
#14458 = DIRECTION ( 'NONE',  ( 1.000000000000000000, 0.000000000000000000, -0.000000000000000000 ) ) ;
#14459 = DIRECTION ( 'NONE',  ( -1.000000000000000000, 0.000000000000000000, 0.000000000000000000 ) ) ;
#14460 = CARTESIAN_POINT ( 'NONE',  ( -16.01409026037699945, 32.68451876144969503, -7.109513113881434698 ) ) ;
#14461 = ORIENTED_EDGE ( 'NONE', *, *, #5277, .F. ) ;
#14462 = CARTESIAN_POINT ( 'NONE',  ( -35.49999999999998579, 10.00000000000000178, -35.00200000000000244 ) ) ;
#14463 = AXIS2_PLACEMENT_3D ( 'NONE', #13925, #195, #1616 ) ;
#14464 = ORIENTED_EDGE ( 'NONE', *, *, #2749, .F. ) ;
#14465 = CARTESIAN_POINT ( 'NONE',  ( 25.17961895204159717, 193.0449522123385577, -27.67906398090707398 ) ) ;
#14466 = DIRECTION ( 'NONE',  ( -1.000000000000000000, -0.000000000000000000, 0.000000000000000000 ) ) ;
#14467 = EDGE_CURVE ( 'NONE', #15051, #2616, #17276, .T. ) ;
#14468 = ORIENTED_EDGE ( 'NONE', *, *, #12250, .T. ) ;
#14469 = EDGE_CURVE ( 'NONE', #5700, #9733, #6463, .T. ) ;
#14470 = ORIENTED_EDGE ( 'NONE', *, *, #15585, .F. ) ;
#14471 = EDGE_CURVE ( 'NONE', #15093, #12155, #1165, .T. ) ;
#14472 = ORIENTED_EDGE ( 'NONE', *, *, #8492, .T. ) ;
#14473 = ADVANCED_FACE ( 'NONE', ( #2589 ), #13201, .T. ) ;
#14474 = CARTESIAN_POINT ( 'NONE',  ( -86.97967542706145139, 149.4008433394086808, -24.40281628369249134 ) ) ;
#14475 = ORIENTED_EDGE ( 'NONE', *, *, #11902, .F. ) ;
#14476 =( NAMED_UNIT ( * ) PLANE_ANGLE_UNIT ( ) SI_UNIT ( $, .RADIAN. ) );
#14477 = CARTESIAN_POINT ( 'NONE',  ( 27.99999999999998224, 9.999999999999998224, 10.00000000000000178 ) ) ;
#14478 = CARTESIAN_POINT ( 'NONE',  ( 26.46257777440031944, 151.4735692324752847, -28.61877689333859465 ) ) ;
#14479 = CARTESIAN_POINT ( 'NONE',  ( 34.42312820349192037, 18.00000000000000000, 9.539278825333477485 ) ) ;
#14480 = CARTESIAN_POINT ( 'NONE',  ( 15.58935622847965163, 125.0306600298041815, 3.338394242842863679 ) ) ;
#14481 = EDGE_LOOP ( 'NONE', ( #6241, #7914, #400, #7556, #15319, #10387 ) ) ;
#14482 = CARTESIAN_POINT ( 'NONE',  ( 27.04079503965286690, 139.2301514590222098, 6.313402927548398047 ) ) ;
#14483 = CARTESIAN_POINT ( 'NONE',  ( -100.0000000000000000, 171.6227766016838245, 0.000000000000000000 ) ) ;
#14484 = CARTESIAN_POINT ( 'NONE',  ( -32.99999999999998579, 10.00000000000000000, -12.99999999999999822 ) ) ;
#14485 = CARTESIAN_POINT ( 'NONE',  ( 33.66231827095856488, 18.00000000000000000, 12.04861179558545636 ) ) ;
#14486 = CARTESIAN_POINT ( 'NONE',  ( -40.00000000000000000, 4.000000000000000000, 30.00000000000000711 ) ) ;
#14487 = EDGE_LOOP ( 'NONE', ( #1781, #6087, #3778, #12493 ) ) ;
#14488 = CARTESIAN_POINT ( 'NONE',  ( -87.05152766480232174, 144.0220640066157785, -18.10843944793621674 ) ) ;
#14489 = CARTESIAN_POINT ( 'NONE',  ( 35.00000000000000000, 196.6227766016838245, 21.54065922853802206 ) ) ;
#14490 = EDGE_LOOP ( 'NONE', ( #14226, #9855 ) ) ;
#14491 = DIRECTION ( 'NONE',  ( 8.673617379884037937E-17, 0.000000000000000000, 1.000000000000000000 ) ) ;
#14492 = CARTESIAN_POINT ( 'NONE',  ( 25.00000000000000000, 196.6227766016838245, 21.54065922853802562 ) ) ;
#14493 = ORIENTED_EDGE ( 'NONE', *, *, #9625, .F. ) ;
#14494 = SHAPE_DEFINITION_REPRESENTATION ( #4325, #9723 ) ;
#14495 = CARTESIAN_POINT ( 'NONE',  ( -81.14508075249469243, 141.7513145237122671, 14.02541974480121567 ) ) ;
#14496 = CARTESIAN_POINT ( 'NONE',  ( 15.45450437963097912, 29.98942126207016301, -13.00000000000000178 ) ) ;
#14497 = CARTESIAN_POINT ( 'NONE',  ( -79.45873686621193599, 140.6457587561385196, -16.29186131275298877 ) ) ;
#14498 = PLANE ( 'NONE',  #6901 ) ;
#14499 = VERTEX_POINT ( 'NONE', #4087 ) ;
#14500 = DIRECTION ( 'NONE',  ( 0.000000000000000000, 0.000000000000000000, -1.000000000000000000 ) ) ;
#14501 = CARTESIAN_POINT ( 'NONE',  ( 27.99999999999998224, 9.999999999999998224, -13.00000000000000000 ) ) ;
#14502 = EDGE_CURVE ( 'NONE', #7894, #13323, #1432, .T. ) ;
#14503 = DIRECTION ( 'NONE',  ( 0.000000000000000000, 0.000000000000000000, -1.000000000000000000 ) ) ;
#14504 = EDGE_CURVE ( 'NONE', #14117, #16962, #14875, .T. ) ;
#14505 = CARTESIAN_POINT ( 'NONE',  ( 34.33044734696805733, 200.7908024820229969, -19.35080275744229894 ) ) ;
#14506 = VERTEX_POINT ( 'NONE', #11868 ) ;
#14507 = ORIENTED_EDGE ( 'NONE', *, *, #15931, .F. ) ;
#14508 = PLANE ( 'NONE',  #3307 ) ;
#14509 = ORIENTED_EDGE ( 'NONE', *, *, #5737, .F. ) ;
#14510 = CARTESIAN_POINT ( 'NONE',  ( -80.00000000000001421, 196.6227766016838245, 0.000000000000000000 ) ) ;
#14511 = ADVANCED_FACE ( 'NONE', ( #6833 ), #1073, .T. ) ;
#14512 = CARTESIAN_POINT ( 'NONE',  ( 10.09659264799822331, 132.0789811519323962, -12.16719622200489681 ) ) ;
#14513 = VERTEX_POINT ( 'NONE', #3817 ) ;
#14514 = CARTESIAN_POINT ( 'NONE',  ( -40.00000000000000000, 0.000000000000000000, 33.00000000000000711 ) ) ;
#14515 = DIRECTION ( 'NONE',  ( -1.000000000000000000, -0.000000000000000000, -0.000000000000000000 ) ) ;
#14516 = CARTESIAN_POINT ( 'NONE',  ( -208.0000000000000853, 170.0678595944000620, -2.693195258168412654 ) ) ;
#14517 = CARTESIAN_POINT ( 'NONE',  ( 34.83135640459488513, 195.3043783022528146, 22.98536326679100128 ) ) ;
#14518 = CARTESIAN_POINT ( 'NONE',  ( 48.00000000000000711, 183.6227766016837961, -5.571800142134975431 ) ) ;
#14519 = DIRECTION ( 'NONE',  ( 1.000000000000000000, -0.000000000000000000, -0.000000000000000000 ) ) ;
#14520 = DIRECTION ( 'NONE',  ( 0.000000000000000000, 8.410780489584519664E-16, -1.000000000000000000 ) ) ;
#14521 = CARTESIAN_POINT ( 'NONE',  ( 34.93420767853316988, 18.00000000000000355, 4.999999999999999112 ) ) ;
#14522 = ORIENTED_EDGE ( 'NONE', *, *, #15425, .F. ) ;
#14523 = DIRECTION ( 'NONE',  ( 0.000000000000000000, 0.8660254037844413721, 0.4999999999999952816 ) ) ;
#14524 = ORIENTED_EDGE ( 'NONE', *, *, #13072, .T. ) ;
#14525 = DIRECTION ( 'NONE',  ( 0.000000000000000000, 0.000000000000000000, 1.000000000000000000 ) ) ;
#14526 = CARTESIAN_POINT ( 'NONE',  ( 0.000000000000000000, 20.00000000000000000, 0.000000000000000000 ) ) ;
#14527 = ORIENTED_EDGE ( 'NONE', *, *, #8876, .F. ) ;
#14528 = EDGE_CURVE ( 'NONE', #2606, #4609, #12397, .T. ) ;
#14529 = CARTESIAN_POINT ( 'NONE',  ( -77.50000000000001421, 196.6227766016838245, 0.000000000000000000 ) ) ;
#14530 = EDGE_CURVE ( 'NONE', #13670, #2134, #11824, .T. ) ;
#14531 = DIRECTION ( 'NONE',  ( -1.000000000000000000, -0.000000000000000000, -0.000000000000000000 ) ) ;
#14532 = ORIENTED_EDGE ( 'NONE', *, *, #3825, .T. ) ;
#14533 = CARTESIAN_POINT ( 'NONE',  ( -5.000000000000000888, 206.6227766016838245, 2.143131898507868248E-15 ) ) ;
#14534 = AXIS2_PLACEMENT_3D ( 'NONE', #10026, #1809, #11624 ) ;
#14535 = ORIENTED_EDGE ( 'NONE', *, *, #17264, .F. ) ;
#14536 = CIRCLE ( 'NONE', #15954, 5.000000000000000888 ) ;
#14537 = CARTESIAN_POINT ( 'NONE',  ( 1.559999999999998943, -0.8660254037844428154, -1.499999999999997780 ) ) ;
#14538 = CARTESIAN_POINT ( 'NONE',  ( 24.91436539010480544, 191.1044234702846154, -26.63673872167001022 ) ) ;
#14539 = DIRECTION ( 'NONE',  ( 0.000000000000000000, 0.8660254037844413721, -0.4999999999999952816 ) ) ;
#14540 = ADVANCED_FACE ( 'NONE', ( #12814 ), #11736, .F. ) ;
#14541 = CARTESIAN_POINT ( 'NONE',  ( -14.07899634757819385, 32.11373924370096233, -10.33209047619764753 ) ) ;
#14542 = ORIENTED_EDGE ( 'NONE', *, *, #5450, .T. ) ;
#14543 = PLANE ( 'NONE',  #1368 ) ;
#14544 = VERTEX_POINT ( 'NONE', #13340 ) ;
#14545 = CARTESIAN_POINT ( 'NONE',  ( 29.55074376293165628, 190.6352453962669813, -29.38582951075080629 ) ) ;
#14546 = CARTESIAN_POINT ( 'NONE',  ( 39.99999999999998579, 0.000000000000000000, 30.00000000000001066 ) ) ;
#14547 = AXIS2_PLACEMENT_3D ( 'NONE', #3203, #14009, #1878 ) ;
#14548 = ORIENTED_EDGE ( 'NONE', *, *, #1030, .F. ) ;
#14549 = CIRCLE ( 'NONE', #12568, 8.000000000000000000 ) ;
#14550 = ORIENTED_EDGE ( 'NONE', *, *, #17042, .T. ) ;
#14551 = ORIENTED_EDGE ( 'NONE', *, *, #13072, .F. ) ;
#14552 = CARTESIAN_POINT ( 'NONE',  ( -84.46470488465458004, 152.6548696709631372, -27.00480063125522889 ) ) ;
#14553 = ORIENTED_EDGE ( 'NONE', *, *, #12480, .T. ) ;
#14554 = SURFACE_STYLE_USAGE ( .BOTH. , #17307 ) ;
#14555 = APPLICATION_CONTEXT ( 'automotive_design' ) ;
#14556 = PLANE ( 'NONE',  #14726 ) ;
#14557 = CARTESIAN_POINT ( 'NONE',  ( -10.71009414332545973, 30.74249144840758063, 14.53036023671900168 ) ) ;
#14558 = AXIS2_PLACEMENT_3D ( 'NONE', #12500, #11425, #4797 ) ;
#14559 = CARTESIAN_POINT ( 'NONE',  ( 33.52233917118052631, 151.4845562501470226, -28.62650789566041354 ) ) ;
#14560 = ADVANCED_FACE ( 'NONE', ( #9257 ), #14308, .F. ) ;
#14561 = CARTESIAN_POINT ( 'NONE',  ( 33.66001102075319551, 18.00000000000000000, 12.05479157725487482 ) ) ;
#14562 = EDGE_CURVE ( 'NONE', #6919, #9322, #10965, .T. ) ;
#14563 = DIRECTION ( 'NONE',  ( -0.000000000000000000, -0.000000000000000000, 1.000000000000000000 ) ) ;
#14564 = VECTOR ( 'NONE', #13010, 1000.000000000000000 ) ;
#14565 = EDGE_CURVE ( 'NONE', #15739, #7241, #17134, .T. ) ;
#14566 = ORIENTED_EDGE ( 'NONE', *, *, #15661, .F. ) ;
#14567 = FACE_OUTER_BOUND ( 'NONE', #11116, .T. ) ;
#14568 = FACE_OUTER_BOUND ( 'NONE', #4062, .T. ) ;
#14569 = CYLINDRICAL_SURFACE ( 'NONE', #7631, 2.500000000000000444 ) ;
#14570 = DIRECTION ( 'NONE',  ( -1.000000000000000000, -0.000000000000000000, -0.000000000000000000 ) ) ;
#14571 = CARTESIAN_POINT ( 'NONE',  ( -15.33310217281973209, 19.99999999999540634, -5.462585411291382975 ) ) ;
#14572 = ORIENTED_EDGE ( 'NONE', *, *, #4576, .F. ) ;
#14573 = CARTESIAN_POINT ( 'NONE',  ( 0.000000000000000000, 0.000000000000000000, 33.00000000000000711 ) ) ;
#14574 = CIRCLE ( 'NONE', #4415, 2.500000000000002220 ) ;
#14575 = CARTESIAN_POINT ( 'NONE',  ( -15.00000000000002132, 90.00000000000000000, -15.00000000000000000 ) ) ;
#14576 = ORIENTED_EDGE ( 'NONE', *, *, #3196, .F. ) ;
#14577 = AXIS2_PLACEMENT_3D ( 'NONE', #12514, #5616, #1800 ) ;
#14578 = FACE_OUTER_BOUND ( 'NONE', #17021, .T. ) ;
#14579 = EDGE_LOOP ( 'NONE', ( #14692, #9684 ) ) ;
#14580 = FILL_AREA_STYLE ('',( #5115 ) ) ;
#14581 = CARTESIAN_POINT ( 'NONE',  ( -84.01578204813917239, 143.6297497249236415, 17.48070775079457917 ) ) ;
#14582 = DIRECTION ( 'NONE',  ( 0.000000000000000000, 0.000000000000000000, 1.000000000000000000 ) ) ;
#14583 = DIRECTION ( 'NONE',  ( -1.000000000000000000, -0.000000000000000000, -0.000000000000000000 ) ) ;
#14584 = EDGE_CURVE ( 'NONE', #2208, #4421, #10311, .T. ) ;
#14585 = CARTESIAN_POINT ( 'NONE',  ( -725.0000000000000000, 134.2062027339443944, 13.00000000000000000 ) ) ;
#14586 = CIRCLE ( 'NONE', #10056, 2.500000000000002220 ) ;
#14587 = AXIS2_PLACEMENT_3D ( 'NONE', #14537, #9131, #4890 ) ;
#14588 = ORIENTED_EDGE ( 'NONE', *, *, #6752, .T. ) ;
#14589 = DIRECTION ( 'NONE',  ( 0.000000000000000000, 0.000000000000000000, -1.000000000000000000 ) ) ;
#14590 = DIRECTION ( 'NONE',  ( -0.000000000000000000, -1.000000000000000000, -0.000000000000000000 ) ) ;
#14591 = AXIS2_PLACEMENT_3D ( 'NONE', #14382, #6150, #16960 ) ;
#14592 = DIRECTION ( 'NONE',  ( 8.673617379884037937E-17, 0.000000000000000000, 1.000000000000000000 ) ) ;
#14593 = CARTESIAN_POINT ( 'NONE',  ( -100.0000000000000000, 144.1839557653416080, 18.33333333333335702 ) ) ;
#14594 = VERTEX_POINT ( 'NONE', #14486 ) ;
#14595 = ORIENTED_EDGE ( 'NONE', *, *, #16042, .F. ) ;
#14596 = DIRECTION ( 'NONE',  ( 2.312964634635742957E-16, -0.000000000000000000, 1.000000000000000000 ) ) ;
#14597 = VERTEX_POINT ( 'NONE', #6607 ) ;
#14598 = CARTESIAN_POINT ( 'NONE',  ( -84.70257449537420769, 150.3543615375532738, -27.79730406782767105 ) ) ;
#14599 = AXIS2_PLACEMENT_3D ( 'NONE', #16564, #357, #4439 ) ;
#14600 = CARTESIAN_POINT ( 'NONE',  ( 11.63249183333955017, 139.6944596454877114, -10.84829254633709539 ) ) ;
#14601 = CIRCLE ( 'NONE', #16871, 2.500000000000002220 ) ;
#14602 = ORIENTED_EDGE ( 'NONE', *, *, #1140, .T. ) ;
#14603 = FACE_OUTER_BOUND ( 'NONE', #2077, .T. ) ;
#14604 = VECTOR ( 'NONE', #9114, 1000.000000000000000 ) ;
#14605 = CARTESIAN_POINT ( 'NONE',  ( -5.000000000000000888, 171.6227766016838245, 0.000000000000000000 ) ) ;
#14606 = EDGE_CURVE ( 'NONE', #16282, #6756, #2440, .T. ) ;
#14607 = DIRECTION ( 'NONE',  ( -0.000000000000000000, -0.000000000000000000, -1.000000000000000000 ) ) ;
#14608 = DIRECTION ( 'NONE',  ( -1.000000000000000000, 0.000000000000000000, 0.000000000000000000 ) ) ;
#14609 = DIRECTION ( 'NONE',  ( 0.000000000000000000, 0.000000000000000000, -1.000000000000000000 ) ) ;
#14610 = CARTESIAN_POINT ( 'NONE',  ( 23.03715179780268585, 17.99999999999999289, -6.069068567132035241 ) ) ;
#14611 = CARTESIAN_POINT ( 'NONE',  ( -95.00000000000000000, 171.6227766016838245, 0.000000000000000000 ) ) ;
#14612 = DIRECTION ( 'NONE',  ( 0.000000000000000000, -0.8660254037844432595, 0.4999999999999919509 ) ) ;
#14613 = CARTESIAN_POINT ( 'NONE',  ( 225.0000000000000000, 89.99999999999997158, 13.00000000000000000 ) ) ;
#14614 = CARTESIAN_POINT ( 'NONE',  ( 25.67867739143054706, 142.4452037501736186, -19.33642647557003613 ) ) ;
#14615 = VERTEX_POINT ( 'NONE', #6428 ) ;
#14616 = CARTESIAN_POINT ( 'NONE',  ( 13.59940502541562246, 130.1762661646492063, -12.36432683418100353 ) ) ;
#14617 = DIRECTION ( 'NONE',  ( -0.000000000000000000, -0.000000000000000000, 1.000000000000000000 ) ) ;
#14618 = AXIS2_PLACEMENT_3D ( 'NONE', #15218, #3095, #13908 ) ;
#14619 = ORIENTED_EDGE ( 'NONE', *, *, #15870, .T. ) ;
#14620 =( GEOMETRIC_REPRESENTATION_CONTEXT ( 3 ) GLOBAL_UNCERTAINTY_ASSIGNED_CONTEXT ( ( #15500 ) ) GLOBAL_UNIT_ASSIGNED_CONTEXT ( ( #3160, #3500, #13963 ) ) REPRESENTATION_CONTEXT ( 'NONE', 'WORKASPACE' ) );
#14621 = DIRECTION ( 'NONE',  ( -1.000000000000000000, 0.000000000000000000, 0.000000000000000000 ) ) ;
#14622 = AXIS2_PLACEMENT_3D ( 'NONE', #13161, #15726, #10502 ) ;
#14623 = CARTESIAN_POINT ( 'NONE',  ( 1.559999999999998943, 0.000000000000000000, 0.000000000000000000 ) ) ;
#14624 = ORIENTED_EDGE ( 'NONE', *, *, #8994, .F. ) ;
#14625 = CARTESIAN_POINT ( 'NONE',  ( -7.379000772444995526, 30.00000000000000000, 15.00000000000000355 ) ) ;
#14626 = CARTESIAN_POINT ( 'NONE',  ( 11.37136921290580460, 130.9041960856249318, 11.49611652308843901 ) ) ;
#14627 = VERTEX_POINT ( 'NONE', #8900 ) ;
#14628 = DIRECTION ( 'NONE',  ( 0.000000000000000000, -1.000000000000000000, -6.123233995736762338E-17 ) ) ;
#14629 = ADVANCED_FACE ( 'NONE', ( #11820, #17225 ), #15901, .F. ) ;
#14630 = EDGE_LOOP ( 'NONE', ( #11389, #8882 ) ) ;
#14631 = AXIS2_PLACEMENT_3D ( 'NONE', #12204, #2900, #1667 ) ;
#14632 = AXIS2_PLACEMENT_3D ( 'NONE', #2316, #731, #3648 ) ;
#14633 = CARTESIAN_POINT ( 'NONE',  ( -75.00000000000002842, 146.6227766016838245, 21.54065922853802562 ) ) ;
#14634 = CARTESIAN_POINT ( 'NONE',  ( 29.40013309498274552, 189.1412428432857951, -27.96613953460096980 ) ) ;
#14635 = CARTESIAN_POINT ( 'NONE',  ( 27.48361012698979877, 126.6227766016837819, -9.278408830390956550E-15 ) ) ;
#14636 = CARTESIAN_POINT ( 'NONE',  ( -11.61061639343520824, 17.99999999999767653, -9.781492982398956926 ) ) ;
#14637 = EDGE_CURVE ( 'NONE', #9979, #5404, #9350, .T. ) ;
#14638 = EDGE_CURVE ( 'NONE', #3748, #8600, #16445, .T. ) ;
#14639 = ORIENTED_EDGE ( 'NONE', *, *, #13957, .F. ) ;
#14640 = DIRECTION ( 'NONE',  ( 0.000000000000000000, 0.000000000000000000, -1.000000000000000000 ) ) ;
#14641 = ORIENTED_EDGE ( 'NONE', *, *, #6788, .F. ) ;
#14642 = CARTESIAN_POINT ( 'NONE',  ( -207.4350753193408821, 174.9908019558275498, -3.998783699268500413 ) ) ;
#14643 = CARTESIAN_POINT ( 'NONE',  ( -87.43654228017076946, 197.7288430733995597, -20.20458554073936597 ) ) ;
#14644 = EDGE_LOOP ( 'NONE', ( #5979, #12045, #12884, #5715 ) ) ;
#14645 = CONICAL_SURFACE ( 'NONE', #8720, 2.499999999999998668, 1.029744260000002187 ) ;
#14646 = ORIENTED_EDGE ( 'NONE', *, *, #3347, .F. ) ;
#14647 = ORIENTED_EDGE ( 'NONE', *, *, #4504, .F. ) ;
#14648 = AXIS2_PLACEMENT_3D ( 'NONE', #1501, #4332, #16552 ) ;
#14649 = CARTESIAN_POINT ( 'NONE',  ( -3.000000000000000888, 204.6227766016838245, 2.020667218593133100E-15 ) ) ;
#14650 = UNCERTAINTY_MEASURE_WITH_UNIT (LENGTH_MEASURE( 1.000000000000000082E-05 ), #12300, 'distance_accuracy_value', 'NONE');
#14651 = ORIENTED_EDGE ( 'NONE', *, *, #6974, .T. ) ;
#14652 = CARTESIAN_POINT ( 'NONE',  ( 0.000000000000000000, 2.000000000000000000, 0.000000000000000000 ) ) ;
#14653 = CARTESIAN_POINT ( 'NONE',  ( -18.15427578192114666, 32.28835078156378557, 6.388283290543781412 ) ) ;
#14654 = DIRECTION ( 'NONE',  ( -0.8571673013836870192, 0.000000000000000000, -0.5150380737757234151 ) ) ;
#14655 = CARTESIAN_POINT ( 'NONE',  ( 35.00000000000000711, 146.6227766016838245, -12.99999999999999822 ) ) ;
#14656 = CARTESIAN_POINT ( 'NONE',  ( 196.0000000000000000, 191.6227766016837677, -5.571800142134975431 ) ) ;
#14657 = VECTOR ( 'NONE', #1204, 1000.000000000000000 ) ;
#14658 = AXIS2_PLACEMENT_3D ( 'NONE', #12274, #3071, #4232 ) ;
#14659 = ORIENTED_EDGE ( 'NONE', *, *, #13821, .T. ) ;
#14660 = CARTESIAN_POINT ( 'NONE',  ( -70.00000000000000000, 143.0439382767972631, -16.49999999999984013 ) ) ;
#14661 = CARTESIAN_POINT ( 'NONE',  ( 22.45772829400591419, 29.90035839190693778, -11.59610751512981253 ) ) ;
#14662 = DIRECTION ( 'NONE',  ( 1.000000000000000000, 0.000000000000000000, 0.000000000000000000 ) ) ;
#14663 = CARTESIAN_POINT ( 'NONE',  ( -95.00000000000000000, 171.6227766016838245, 0.000000000000000000 ) ) ;
#14664 = CARTESIAN_POINT ( 'NONE',  ( 19.36310082087489803, 29.94084738964976111, 13.97143931599698874 ) ) ;
#14665 = EDGE_LOOP ( 'NONE', ( #14246, #15400, #8968, #9413 ) ) ;
#14666 = CARTESIAN_POINT ( 'NONE',  ( -87.50000000000005684, 146.0571958828608388, -20.88424858573642595 ) ) ;
#14667 = AXIS2_PLACEMENT_3D ( 'NONE', #13720, #2917, #9639 ) ;
#14668 = DIRECTION ( 'NONE',  ( -1.000000000000000000, 0.000000000000000000, 0.000000000000000000 ) ) ;
#14669 = EDGE_CURVE ( 'NONE', #5075, #12878, #6872, .T. ) ;
#14670 = EDGE_CURVE ( 'NONE', #6919, #13751, #139, .T. ) ;
#14671 = ORIENTED_EDGE ( 'NONE', *, *, #9211, .F. ) ;
#14672 = CARTESIAN_POINT ( 'NONE',  ( -32.65377812985506978, 100.8098204658883361, -4.906772862994290385 ) ) ;
#14674 = CARTESIAN_POINT ( 'NONE',  ( 37.50000000000000711, 146.6227766016838245, -35.00200000000000244 ) ) ;
#14673 = VECTOR ( 'NONE', #12696, 1000.000000000000000 ) ;
#14675 = ORIENTED_EDGE ( 'NONE', *, *, #4139, .T. ) ;
#14676 = DIRECTION ( 'NONE',  ( 0.000000000000000000, 0.000000000000000000, -1.000000000000000000 ) ) ;
#14677 = CARTESIAN_POINT ( 'NONE',  ( -27.98221281347037959, 18.00000000000000355, 4.999999999999999112 ) ) ;
#14678 = CARTESIAN_POINT ( 'NONE',  ( -153.0000000000000284, 171.6227766016838245, 0.000000000000000000 ) ) ;
#14679 = CARTESIAN_POINT ( 'NONE',  ( -187.6513770290094669, 171.1853623553243722, -0.7576236986489900405 ) ) ;
#14680 = VERTEX_POINT ( 'NONE', #58 ) ;
#14681 = CARTESIAN_POINT ( 'NONE',  ( -197.9999999999999716, 171.6227766016838245, 14.16444493696511486 ) ) ;
#14682 = AXIS2_PLACEMENT_3D ( 'NONE', #8120, #13532, #16110 ) ;
#14683 = CARTESIAN_POINT ( 'NONE',  ( 1.559999999999998943, 0.8660254037844428154, -1.499999999999997780 ) ) ;
#14684 = VECTOR ( 'NONE', #11872, 1000.000000000000000 ) ;
#14685 = DIRECTION ( 'NONE',  ( -0.000000000000000000, -0.000000000000000000, 1.000000000000000000 ) ) ;
#14686 = VECTOR ( 'NONE', #3609, 1000.000000000000000 ) ;
#14687 = ORIENTED_EDGE ( 'NONE', *, *, #10068, .F. ) ;
#14688 = CARTESIAN_POINT ( 'NONE',  ( 7.535032041485008492, 142.5209969262061804, -19.44444444359253410 ) ) ;
#14689 = ADVANCED_FACE ( 'NONE', ( #2712 ), #2628, .F. ) ;
#14690 = EDGE_CURVE ( 'NONE', #12127, #5890, #4205, .T. ) ;
#14691 = EDGE_CURVE ( 'NONE', #2797, #1250, #5917, .T. ) ;
#14692 = ORIENTED_EDGE ( 'NONE', *, *, #5123, .F. ) ;
#14693 = CARTESIAN_POINT ( 'NONE',  ( -85.55727518495883999, 148.9119151679986999, -26.63478011418837710 ) ) ;
#14694 = EDGE_CURVE ( 'NONE', #14615, #6145, #17508, .T. ) ;
#14695 = CARTESIAN_POINT ( 'NONE',  ( 14.09268385650717015, 127.7503171827756034, -9.071975374176082241 ) ) ;
#14696 = AXIS2_PLACEMENT_3D ( 'NONE', #1506, #1242, #16297 ) ;
#14697 = EDGE_LOOP ( 'NONE', ( #5865, #208 ) ) ;
#14698 = CARTESIAN_POINT ( 'NONE',  ( 196.0000000000000000, 187.6227766016837961, 12.50000337241049309 ) ) ;
#14699 = DIRECTION ( 'NONE',  ( 0.000000000000000000, -0.8660254037844432595, 0.4999999999999919509 ) ) ;
#14700 = AXIS2_PLACEMENT_3D ( 'NONE', #16918, #4795, #3462 ) ;
#14701 = CARTESIAN_POINT ( 'NONE',  ( -151.0000000000000284, 171.6227766016838245, 0.000000000000000000 ) ) ;
#14702 = DIRECTION ( 'NONE',  ( 0.9961946980917465444, 0.08715574274764831264, 0.000000000000000000 ) ) ;
#14703 = CARTESIAN_POINT ( 'NONE',  ( 33.88556156013721932, 18.00000000000000000, -11.42442012027869858 ) ) ;
#14704 =( BOUNDED_CURVE ( )  B_SPLINE_CURVE ( 3, ( #12344, #12253, #47, #2954 ),
 .UNSPECIFIED., .F., .F. ) 
 B_SPLINE_CURVE_WITH_KNOTS ( ( 4, 4 ),
 ( 3.141592653589792672, 4.712388980384690562 ),
 .UNSPECIFIED. ) 
 CURVE ( )  GEOMETRIC_REPRESENTATION_ITEM ( )  RATIONAL_B_SPLINE_CURVE ( ( 1.000000000000000000, 0.8047378541243646044, 0.8047378541243646044, 1.000000000000000000 ) ) 
 REPRESENTATION_ITEM ( '' )  );
#14705 = CARTESIAN_POINT ( 'NONE',  ( 21.98114852961722576, 18.00000000000000000, -23.72829316725777815 ) ) ;
#14706 = DIRECTION ( 'NONE',  ( -1.000000000000000000, -0.000000000000000000, -0.000000000000000000 ) ) ;
#14707 = PLANE ( 'NONE',  #13834 ) ;
#14708 = CARTESIAN_POINT ( 'NONE',  ( -208.1430079281944074, 176.3671987152221448, 3.647967993167786194 ) ) ;
#14709 = CYLINDRICAL_SURFACE ( 'NONE', #2123, 27.69059892324149530 ) ;
#14710 = EDGE_LOOP ( 'NONE', ( #12798, #17162 ) ) ;
#14711 = DIRECTION ( 'NONE',  ( 1.000000000000000000, 6.938893903907228378E-16, -0.000000000000000000 ) ) ;
#14712 = VECTOR ( 'NONE', #12006, 1000.000000000000000 ) ;
#14713 = AXIS2_PLACEMENT_3D ( 'NONE', #10767, #16178, #15353 ) ;
#14714 = ORIENTED_EDGE ( 'NONE', *, *, #16570, .T. ) ;
#14715 = ADVANCED_FACE ( 'NONE', ( #1477 ), #5541, .T. ) ;
#14716 = DIRECTION ( 'NONE',  ( -1.000000000000000000, -0.000000000000000000, -0.000000000000000000 ) ) ;
#14717 = AXIS2_PLACEMENT_3D ( 'NONE', #5622, #128, #8348 ) ;
#14718 = DIRECTION ( 'NONE',  ( 0.000000000000000000, 0.000000000000000000, 1.000000000000000000 ) ) ;
#14719 = ORIENTED_EDGE ( 'NONE', *, *, #8828, .T. ) ;
#14720 = CARTESIAN_POINT ( 'NONE',  ( -43.00000000000000000, 138.6227766016838245, 0.000000000000000000 ) ) ;
#14721 = CARTESIAN_POINT ( 'NONE',  ( 26.46962346220079709, 139.5657242622003480, 7.835998493359402239 ) ) ;
#14722 = ORIENTED_EDGE ( 'NONE', *, *, #4926, .F. ) ;
#14723 = CARTESIAN_POINT ( 'NONE',  ( 18.15033819753324806, 29.95689775512239805, 14.47405640211066213 ) ) ;
#14724 = TOROIDAL_SURFACE ( 'NONE', #14713, 21.61734737250326077, 2.000000000000000000 ) ;
#14725 = ORIENTED_EDGE ( 'NONE', *, *, #1969, .T. ) ;
#14726 = AXIS2_PLACEMENT_3D ( 'NONE', #13236, #12436, #14745 ) ;
#14727 = CARTESIAN_POINT ( 'NONE',  ( -208.1430079281944074, 176.3671987152221448, 0.000000000000000000 ) ) ;
#14728 = CARTESIAN_POINT ( 'NONE',  ( -725.0000000000000000, 30.00000000000000000, 25.00000000000000000 ) ) ;
#14729 = LINE ( 'NONE', #6668, #7956 ) ;
#14730 = CARTESIAN_POINT ( 'NONE',  ( -25.81900932159184592, 18.00000000000000000, -13.95463872937486194 ) ) ;
#14731 = VERTEX_POINT ( 'NONE', #8013 ) ;
#14732 = CARTESIAN_POINT ( 'NONE',  ( 33.65445145306948405, 150.0509117818997424, 24.97535314687242902 ) ) ;
#14733 = EDGE_CURVE ( 'NONE', #5007, #8095, #2036, .T. ) ;
#14734 = ORIENTED_EDGE ( 'NONE', *, *, #15386, .F. ) ;
#14735 = ADVANCED_FACE ( 'NONE', ( #10770 ), #5633, .T. ) ;
#14736 = CARTESIAN_POINT ( 'NONE',  ( -77.20631483639103010, 189.6403081819231033, -27.64877209012309578 ) ) ;
#14737 = CARTESIAN_POINT ( 'NONE',  ( -86.41998248565997187, 200.5275637277236171, -15.94334347237690785 ) ) ;
#14738 = ORIENTED_EDGE ( 'NONE', *, *, #9307, .T. ) ;
#14739 = ORIENTED_EDGE ( 'NONE', *, *, #10708, .F. ) ;
#14740 = EDGE_LOOP ( 'NONE', ( #17277, #13221, #9280, #4040 ) ) ;
#14741 = CARTESIAN_POINT ( 'NONE',  ( 15.00000000000000000, 206.6227766016838245, 2.143131898507868248E-15 ) ) ;
#14742 = EDGE_CURVE ( 'NONE', #5523, #6530, #824, .T. ) ;
#14743 = VERTEX_POINT ( 'NONE', #13778 ) ;
#14744 = CARTESIAN_POINT ( 'NONE',  ( -80.00000000000001421, 196.6227766016838245, -18.75000000000000355 ) ) ;
#14745 = DIRECTION ( 'NONE',  ( 1.000000000000000000, 0.000000000000000000, -0.000000000000000000 ) ) ;
#14746 = CARTESIAN_POINT ( 'NONE',  ( -14.60673078645093703, 31.57037919282903360, 12.49506642855920724 ) ) ;
#14747 = CARTESIAN_POINT ( 'NONE',  ( 26.63786622865510267, 151.5968920417501806, -28.70510347301450693 ) ) ;
#14748 = AXIS2_PLACEMENT_3D ( 'NONE', #14206, #7808, #15783 ) ;
#14749 = CARTESIAN_POINT ( 'NONE',  ( 49.99999999999998579, 175.6227766016838530, -16.92820660268601429 ) ) ;
#14750 = CARTESIAN_POINT ( 'NONE',  ( -77.43519705649855212, 150.9309764409412651, 25.70786830908635068 ) ) ;
#14751 = ORIENTED_EDGE ( 'NONE', *, *, #2235, .T. ) ;
#14752 = CARTESIAN_POINT ( 'NONE',  ( -85.93249065294895672, 197.5381456772451543, -23.52581655030730445 ) ) ;
#14753 = CARTESIAN_POINT ( 'NONE',  ( 24.29886777166023393, 29.87658293154515832, -8.524716167024733338 ) ) ;
#14754 = DIRECTION ( 'NONE',  ( 0.000000000000000000, 0.000000000000000000, 1.000000000000000000 ) ) ;
#14755 = FACE_OUTER_BOUND ( 'NONE', #6335, .T. ) ;
#14756 = CARTESIAN_POINT ( 'NONE',  ( -87.50000000000004263, 196.6227766016838245, -35.00200000000000244 ) ) ;
#14757 = VERTEX_POINT ( 'NONE', #7048 ) ;
#14758 = DIRECTION ( 'NONE',  ( -1.000000000000000000, 0.000000000000000000, 0.000000000000000000 ) ) ;
#14759 = CARTESIAN_POINT ( 'NONE',  ( -48.00000000000000000, 171.6227766016838245, 0.000000000000000000 ) ) ;
#14760 = CARTESIAN_POINT ( 'NONE',  ( -27.99999999999998224, 10.00000000000000000, -35.00000000000000000 ) ) ;
#14761 = ORIENTED_EDGE ( 'NONE', *, *, #112, .F. ) ;
#14762 = ADVANCED_FACE ( 'NONE', ( #6698 ), #15513, .T. ) ;
#14763 = ORIENTED_EDGE ( 'NONE', *, *, #1538, .T. ) ;
#14764 =( NAMED_UNIT ( * ) PLANE_ANGLE_UNIT ( ) SI_UNIT ( $, .RADIAN. ) );
#14765 = CARTESIAN_POINT ( 'NONE',  ( 39.99999999999998579, 8.000000000000000000, -29.99999999999999645 ) ) ;
#14766 = DIRECTION ( 'NONE',  ( 8.673617379884037937E-17, 0.000000000000000000, 1.000000000000000000 ) ) ;
#14767 = CARTESIAN_POINT ( 'NONE',  ( -85.73950972639505608, 144.8396561671642928, -22.53731575973596790 ) ) ;
#14768 = CARTESIAN_POINT ( 'NONE',  ( -26.10410744458348020, 20.00000000000000000, 13.37721135299797659 ) ) ;
#14769 = ORIENTED_EDGE ( 'NONE', *, *, #16461, .T. ) ;
#14770 = CARTESIAN_POINT ( 'NONE',  ( 39.99999999999998579, 20.00000000000000000, 30.00000000000001066 ) ) ;
#14771 = LINE ( 'NONE', #14848, #1970 ) ;
#14772 = EDGE_CURVE ( 'NONE', #12728, #1301, #8451, .T. ) ;
#14773 = CARTESIAN_POINT ( 'NONE',  ( -45.00000000000000711, 171.6227766016838245, 0.000000000000000000 ) ) ;
#14774 = CARTESIAN_POINT ( 'NONE',  ( 35.49999999999998579, 9.999999999999998224, -28.00000000000001066 ) ) ;
#14775 = ORIENTED_EDGE ( 'NONE', *, *, #14742, .T. ) ;
#14776 = CARTESIAN_POINT ( 'NONE',  ( 26.76721132277178228, 137.4464968366854407, -7.553125767360616472 ) ) ;
#14777 = VERTEX_POINT ( 'NONE', #3150 ) ;
#14778 = CARTESIAN_POINT ( 'NONE',  ( -85.41162126782658959, 149.2402085794912807, -26.91083197558417339 ) ) ;
#14779 = CARTESIAN_POINT ( 'NONE',  ( 15.12922779335904977, 126.1891464972476911, -7.145555214655046505 ) ) ;
#14780 = VERTEX_POINT ( 'NONE', #4391 ) ;
#14781 = PLANE ( 'NONE',  #16967 ) ;
#14782 = CARTESIAN_POINT ( 'NONE',  ( 196.0000000000000000, 191.6227766016837677, 5.571800142134975431 ) ) ;
#14783 = CARTESIAN_POINT ( 'NONE',  ( 34.98026256913478704, 196.1036955441147995, 22.13227804827259959 ) ) ;
#14784 = CARTESIAN_POINT ( 'NONE',  ( 17.55923266082603007, 17.99999999999999645, -24.87049340120105612 ) ) ;
#14785 = CARTESIAN_POINT ( 'NONE',  ( 34.42312820349192037, 18.00000000000000000, -9.539278825333477485 ) ) ;
#14786 = CARTESIAN_POINT ( 'NONE',  ( -48.00000000000000000, 154.3022685259950038, 9.999999999999900524 ) ) ;
#14787 = DIRECTION ( 'NONE',  ( 0.000000000000000000, 1.000000000000000000, 1.224646799147353207E-16 ) ) ;
#14788 = ADVANCED_FACE ( 'NONE', ( #16701 ), #8458, .F. ) ;
#14789 = EDGE_CURVE ( 'NONE', #9130, #2208, #12614, .T. ) ;
#14790 = DIRECTION ( 'NONE',  ( -0.000000000000000000, -0.000000000000000000, 1.000000000000000000 ) ) ;
#14791 = EDGE_CURVE ( 'NONE', #13335, #5075, #5627, .T. ) ;
#14792 = CARTESIAN_POINT ( 'NONE',  ( 24.00000000000000355, 146.6227766016838245, -24.49489742783179480 ) ) ;
#14793 = EDGE_LOOP ( 'NONE', ( #83, #15360, #14986, #2078 ) ) ;
#14794 = LINE ( 'NONE', #12046, #12120 ) ;
#14795 = ORIENTED_EDGE ( 'NONE', *, *, #13389, .T. ) ;
#14796 = DIRECTION ( 'NONE',  ( -0.000000000000000000, -0.000000000000000000, -1.000000000000000000 ) ) ;
#14797 = FACE_BOUND ( 'NONE', #2891, .T. ) ;
#14798 = VERTEX_POINT ( 'NONE', #11287 ) ;
#14799 = CARTESIAN_POINT ( 'NONE',  ( -11.67692690462290273, 19.99999999999766587, 12.94410612366815272 ) ) ;
#14800 = CARTESIAN_POINT ( 'NONE',  ( 14.46714703242257904, 138.5709836085849531, 4.391619799164913296 ) ) ;
#14801 = ORIENTED_EDGE ( 'NONE', *, *, #10509, .F. ) ;
#14802 = CARTESIAN_POINT ( 'NONE',  ( 16.23418548573199516, 29.98246013044581915, 14.93677958672484785 ) ) ;
#14803 =( BOUNDED_SURFACE ( )  B_SPLINE_SURFACE ( 3, 2, ( 
 ( #2321, #15681, #14199 ),
 ( #4636, #16941, #649 ),
 ( #3563, #4887, #14115 ),
 ( #986, #15429, #4974 ),
 ( #9047, #11688, #8706 ),
 ( #11529, #8955, #14455 ),
 ( #2143, #6046, #10205 ),
 ( #14365, #3305, #12953 ),
 ( #11359, #10110, #912 ),
 ( #17023, #17103, #10367 ),
 ( #2236, #7712, #10015 ),
 ( #11619, #7543, #7629 ),
 ( #13120, #6221, #13043 ),
 ( #10278, #1977, #15777 ),
 ( #6300, #15601, #11439 ),
 ( #7381, #12779, #16850 ),
 ( #3479, #15518, #4722 ),
 ( #8793, #2060, #738 ),
 ( #6134, #14274, #828 ),
 ( #4096, #10641, #9399 ),
 ( #24, #5067, #14723 ),
 ( #16228, #14887, #10733 ),
 ( #10817, #17192, #11968 ),
 ( #3926, #9476, #15951 ),
 ( #13478, #9220, #6663 ),
 ( #3830, #10462, #14802 ),
 ( #5428, #10545, #17285 ),
 ( #6485, #2502, #5239 ) ),
 .UNSPECIFIED., .F., .F., .F. ) 
 B_SPLINE_SURFACE_WITH_KNOTS ( ( 4, 2, 2, 2, 2, 2, 2, 2, 2, 2, 2, 2, 2, 4 ),
 ( 3, 3 ),
 ( 0.01342997177288654184, 0.01733910390705691029, 0.01929366997414209278, 0.02124823604122727527, 0.02515736817539764372, 0.02711193424248282968, 0.02906650030956801217, 0.03297563244373838409, 0.03493019851082356658, 0.03688476457790874907, 0.03883933064499393156, 0.03981661367853651934, 0.04079389671207911405, 0.04470302884624948597 ),
 ( 0.000000000000000000, 1.000000000000000000 ),
 .UNSPECIFIED. ) 
 GEOMETRIC_REPRESENTATION_ITEM ( )  RATIONAL_B_SPLINE_SURFACE ( (
 ( 1.000000000000000000, 0.7117435966472906994, 1.000000000000000000),
 ( 1.000000000000000000, 0.7117434842622788471, 1.000000000000000000),
 ( 1.000000000000000000, 0.7117144184576317256, 1.000000000000000000),
 ( 1.000000000000000000, 0.7116285301813536357, 1.000000000000000000),
 ( 1.000000000000000000, 0.7115928256594988843, 1.000000000000000000),
 ( 1.000000000000000000, 0.7115068832447583036, 1.000000000000000000),
 ( 1.000000000000000000, 0.7114564033771691998, 1.000000000000000000),
 ( 1.000000000000000000, 0.7112861117250206533, 1.000000000000000000),
 ( 1.000000000000000000, 0.7111469280185451769, 1.000000000000000000),
 ( 1.000000000000000000, 0.7108993804763810154, 1.000000000000000000),
 ( 1.000000000000000000, 0.7108100171490498997, 1.000000000000000000),
 ( 1.000000000000000000, 0.7106191415567917335, 1.000000000000000000),
 ( 1.000000000000000000, 0.7105185320923617098, 1.000000000000000000),
 ( 1.000000000000000000, 0.7102014790723296667, 1.000000000000000000),
 ( 1.000000000000000000, 0.7099699576741209661, 1.000000000000000000),
 ( 1.000000000000000000, 0.7095909300314675594, 1.000000000000000000),
 ( 1.000000000000000000, 0.7094593121158619953, 1.000000000000000000),
 ( 1.000000000000000000, 0.7091910831478104305, 1.000000000000000000),
 ( 1.000000000000000000, 0.7090537746377190143, 1.000000000000000000),
 ( 1.000000000000000000, 0.7087727591781516345, 1.000000000000000000),
 ( 1.000000000000000000, 0.7086290523620303317, 1.000000000000000000),
 ( 1.000000000000000000, 0.7084085592173990920, 1.000000000000000000),
 ( 1.000000000000000000, 0.7083342380282030559, 1.000000000000000000),
 ( 1.000000000000000000, 0.7081839094108949295, 1.000000000000000000),
 ( 1.000000000000000000, 0.7081077478408516201, 1.000000000000000000),
 ( 1.000000000000000000, 0.7077267031859736379, 1.000000000000000000),
 ( 1.000000000000000000, 0.7074184602292508117, 1.000000000000000000),
 ( 1.000000000000000000, 0.7071067811865475727, 1.000000000000000000) ) ) 
 REPRESENTATION_ITEM ( '' )  SURFACE ( )  );
#14804 = ORIENTED_EDGE ( 'NONE', *, *, #8829, .F. ) ;
#14805 = PLANE ( 'NONE',  #17436 ) ;
#14806 = CARTESIAN_POINT ( 'NONE',  ( 15.58935537591275811, 125.0306660307430349, -3.338448778865417577 ) ) ;
#14807 = DIRECTION ( 'NONE',  ( 1.000000000000000000, 0.000000000000000000, 0.000000000000000000 ) ) ;
#14808 = DIRECTION ( 'NONE',  ( 0.000000000000000000, 0.5000000000000011102, -0.8660254037844379305 ) ) ;
#14809 = ORIENTED_EDGE ( 'NONE', *, *, #9339, .F. ) ;
#14810 = CARTESIAN_POINT ( 'NONE',  ( 34.83193525651911671, 147.9395323639054141, 22.98372036160736798 ) ) ;
#14811 = ORIENTED_EDGE ( 'NONE', *, *, #12564, .F. ) ;
#14812 = CARTESIAN_POINT ( 'NONE',  ( -85.62055130997418928, 191.6508168144185902, -26.22852547856965444 ) ) ;
#14813 = CARTESIAN_POINT ( 'NONE',  ( -27.99999999999998224, 10.00000000000000000, 10.00000000000000178 ) ) ;
#14814 = ORIENTED_EDGE ( 'NONE', *, *, #6974, .F. ) ;
#14815 = ORIENTED_EDGE ( 'NONE', *, *, #11755, .T. ) ;
#14816 = ORIENTED_EDGE ( 'NONE', *, *, #16570, .F. ) ;
#14817 = CIRCLE ( 'NONE', #11690, 6.000000000000001776 ) ;
#14818 = DIRECTION ( 'NONE',  ( -0.000000000000000000, -0.000000000000000000, -1.000000000000000000 ) ) ;
#14819 = VERTEX_POINT ( 'NONE', #753 ) ;
#14820 = PRODUCT_CONTEXT ( 'NONE', #14001, 'mechanical' ) ;
#14821 = DIRECTION ( 'NONE',  ( -1.000000000000000000, -0.000000000000000000, 0.000000000000000000 ) ) ;
#14822 = EDGE_CURVE ( 'NONE', #1044, #7220, #8723, .T. ) ;
#14823 = CARTESIAN_POINT ( 'NONE',  ( 34.93420767853316988, 30.00000000000000000, 4.999999999999999112 ) ) ;
#14824 = CARTESIAN_POINT ( 'NONE',  ( 22.42614717998981178, 29.85190128815754917, -7.820018500632365033 ) ) ;
#14825 = CARTESIAN_POINT ( 'NONE',  ( 0.000000000000000000, 0.000000000000000000, 0.000000000000000000 ) ) ;
#14826 = CARTESIAN_POINT ( 'NONE',  ( -81.55625601990109885, 151.3901271056993210, 26.07015880384263085 ) ) ;
#14827 = ORIENTED_EDGE ( 'NONE', *, *, #10226, .F. ) ;
#14828 = CARTESIAN_POINT ( 'NONE',  ( -82.59122206075636541, 202.0384121146825862, -17.31838511551979565 ) ) ;
#14830 = CARTESIAN_POINT ( 'NONE',  ( 9.788850454972870097, 132.9181049171561995, 14.40474131580982231 ) ) ;
#14829 = AXIS2_PLACEMENT_3D ( 'NONE', #641, #8331, #7104 ) ;
#14831 = CARTESIAN_POINT ( 'NONE',  ( 19.49710218362280045, 17.99999999999999289, 24.48336163992366465 ) ) ;
#14832 = DIRECTION ( 'NONE',  ( 0.000000000000000000, 0.000000000000000000, -1.000000000000000000 ) ) ;
#14833 = PLANE ( 'NONE',  #15424 ) ;
#14834 = ADVANCED_FACE ( 'NONE', ( #12709, #11108 ), #4571, .T. ) ;
#14835 = DIRECTION ( 'NONE',  ( -0.000000000000000000, -0.000000000000000000, 1.000000000000000000 ) ) ;
#14836 = ORIENTED_EDGE ( 'NONE', *, *, #11806, .F. ) ;
#14837 = DIRECTION ( 'NONE',  ( 0.000000000000000000, 0.000000000000000000, -1.000000000000000000 ) ) ;
#14838 = CIRCLE ( 'NONE', #7205, 2.500000000000000000 ) ;
#14839 = EDGE_LOOP ( 'NONE', ( #10307, #6932, #5935, #6437 ) ) ;
#14840 = CARTESIAN_POINT ( 'NONE',  ( -30.49999999999998224, 10.00000000000000000, 0.000000000000000000 ) ) ;
#14841 = EDGE_CURVE ( 'NONE', #243, #16962, #17213, .T. ) ;
#14842 = CARTESIAN_POINT ( 'NONE',  ( -40.00000000000000000, 4.000000000000000000, 33.00000000000000711 ) ) ;
#14843 = CARTESIAN_POINT ( 'NONE',  ( -40.00000000000000000, 8.000000000000000000, -30.00000000000000355 ) ) ;
#14844 = CARTESIAN_POINT ( 'NONE',  ( -14.54670497998687217, 20.00000000000000000, 23.76610458325320607 ) ) ;
#14845 = VERTEX_POINT ( 'NONE', #16867 ) ;
#14846 = CARTESIAN_POINT ( 'NONE',  ( 39.99999999999998579, 0.000000000000000000, 39.99999999999998579 ) ) ;
#14847 = EDGE_CURVE ( 'NONE', #1902, #10173, #14131, .T. ) ;
#14848 = CARTESIAN_POINT ( 'NONE',  ( 39.99999999999998579, 20.00000000000000000, 30.00000000000001066 ) ) ;
#14849 = CARTESIAN_POINT ( 'NONE',  ( -5.000000000000000888, 171.6227766016838245, -20.00000000000000355 ) ) ;
#14850 = ADVANCED_FACE ( 'NONE', ( #1737 ), #15444, .F. ) ;
#14851 = SURFACE_SIDE_STYLE ('',( #4067 ) ) ;
#14852 = ADVANCED_FACE ( 'NONE', ( #12530 ), #1814, .T. ) ;
#14853 = VECTOR ( 'NONE', #17515, 1000.000000000000000 ) ;
#14854 = VECTOR ( 'NONE', #3165, 1000.000000000000114 ) ;
#14855 = CIRCLE ( 'NONE', #13164, 30.00000000000000000 ) ;
#14856 = CARTESIAN_POINT ( 'NONE',  ( 17.14535223351611748, 126.3036220646326910, -7.355580850454368047 ) ) ;
#14857 = ORIENTED_EDGE ( 'NONE', *, *, #11731, .T. ) ;
#14858 = PLANE ( 'NONE',  #13488 ) ;
#14859 = CARTESIAN_POINT ( 'NONE',  ( 40.00000000000000711, 171.6227766016838245, 0.000000000000000000 ) ) ;
#14860 = ORIENTED_EDGE ( 'NONE', *, *, #12456, .T. ) ;
#14861 = EDGE_CURVE ( 'NONE', #14086, #3946, #13548, .T. ) ;
#14862 = DIRECTION ( 'NONE',  ( 0.000000000000000000, 0.000000000000000000, -1.000000000000000000 ) ) ;
#14863 = CARTESIAN_POINT ( 'NONE',  ( -83.36338409889501122, 191.6363561590498250, -28.71510896997970264 ) ) ;
#14864 = CIRCLE ( 'NONE', #4130, 2.499999999999999112 ) ;
#14865 = CIRCLE ( 'NONE', #16857, 2.500000000000002220 ) ;
#14866 = DIRECTION ( 'NONE',  ( 0.000000000000000000, 0.000000000000000000, 1.000000000000000000 ) ) ;
#14867 = CARTESIAN_POINT ( 'NONE',  ( 34.89574631506663849, 195.5720014495397265, 22.70655749026626680 ) ) ;
#14868 = CARTESIAN_POINT ( 'NONE',  ( 14.93242934743711992, 18.00000000000000355, -25.00000000000000000 ) ) ;
#14869 = CARTESIAN_POINT ( 'NONE',  ( 18.47042353409679194, 29.92915261368834479, -12.18054208566702279 ) ) ;
#14870 = CARTESIAN_POINT ( 'NONE',  ( 196.0000000000000000, 175.6227766016838530, 19.42820660268601074 ) ) ;
#14871 = DIRECTION ( 'NONE',  ( -1.000000000000000000, 0.000000000000000000, 0.000000000000000000 ) ) ;
#14872 = PLANE ( 'NONE',  #850 ) ;
#14873 =( NAMED_UNIT ( * ) PLANE_ANGLE_UNIT ( ) SI_UNIT ( $, .RADIAN. ) );
#14874 = ORIENTED_EDGE ( 'NONE', *, *, #575, .F. ) ;
#14875 = LINE ( 'NONE', #2756, #12393 ) ;
#14876 = ORIENTED_EDGE ( 'NONE', *, *, #2631, .T. ) ;
#14877 = CYLINDRICAL_SURFACE ( 'NONE', #9762, 20.00000000000000355 ) ;
#14878 = CIRCLE ( 'NONE', #14320, 4.999999999999997335 ) ;
#14879 = CIRCLE ( 'NONE', #7245, 1.000000000000000888 ) ;
#14880 = CARTESIAN_POINT ( 'NONE',  ( -50.00000000000000000, 171.6227766016838245, -2.602085213965210642E-15 ) ) ;
#14881 = ORIENTED_EDGE ( 'NONE', *, *, #11083, .F. ) ;
#14882 = DIRECTION ( 'NONE',  ( 0.000000000000000000, -1.000000000000000000, 0.000000000000000000 ) ) ;
#14883 = CARTESIAN_POINT ( 'NONE',  ( 6.134011831684059501, 134.2062027339443944, -24.99999999999999645 ) ) ;
#14884 = ADVANCED_FACE ( 'NONE', ( #8627 ), #14213, .T. ) ;
#14885 = ORIENTED_EDGE ( 'NONE', *, *, #5052, .F. ) ;
#14886 = EDGE_CURVE ( 'NONE', #8470, #6189, #7042, .T. ) ;
#14887 = CARTESIAN_POINT ( 'NONE',  ( 17.69056612348262192, 20.00000000000056488, 14.65191630173004711 ) ) ;
#14888 = EDGE_CURVE ( 'NONE', #8372, #1583, #16784, .T. ) ;
#14889 = ORIENTED_EDGE ( 'NONE', *, *, #5640, .T. ) ;
#14890 = DIRECTION ( 'NONE',  ( -0.000000000000000000, -0.000000000000000000, -1.000000000000000000 ) ) ;
#14891 = DIRECTION ( 'NONE',  ( 1.000000000000000000, 0.000000000000000000, 0.000000000000000000 ) ) ;
#14892 = CARTESIAN_POINT ( 'NONE',  ( -208.0000000000000853, 174.7326106162513497, 0.000000000000000000 ) ) ;
#14893 = AXIS2_PLACEMENT_3D ( 'NONE', #16860, #17447, #746 ) ;
#14894 = CARTESIAN_POINT ( 'NONE',  ( 27.48361012698976324, 138.6227766016838245, 1.226160068396871639 ) ) ;
#14895 = AXIS2_PLACEMENT_3D ( 'NONE', #6177, #4769, #4854 ) ;
#14896 = ORIENTED_EDGE ( 'NONE', *, *, #11396, .T. ) ;
#14897 = CARTESIAN_POINT ( 'NONE',  ( -5.000000000000000888, 171.6227766016838245, 20.00000000000000355 ) ) ;
#14898 =( REPRESENTATION_RELATIONSHIP ('NONE','NONE', #9723, #16423 ) REPRESENTATION_RELATIONSHIP_WITH_TRANSFORMATION ( #6780 )SHAPE_REPRESENTATION_RELATIONSHIP( ) );
#14899 = VERTEX_POINT ( 'NONE', #10033 ) ;
#14900 = CARTESIAN_POINT ( 'NONE',  ( -75.53529511534544838, 190.5906835324044550, -27.00480063125522889 ) ) ;
#14901 = PLANE ( 'NONE',  #3569 ) ;
#14902 = CARTESIAN_POINT ( 'NONE',  ( -14.96200682865387854, 32.37632742624003157, -9.274234733431431010 ) ) ;
#14903 = VERTEX_POINT ( 'NONE', #15535 ) ;
#14904 = ORIENTED_EDGE ( 'NONE', *, *, #968, .F. ) ;
#14905 = ADVANCED_FACE ( 'NONE', ( #8810 ), #7876, .F. ) ;
#14906 = EDGE_CURVE ( 'NONE', #457, #2935, #16015, .T. ) ;
#14907 = AXIS2_PLACEMENT_3D ( 'NONE', #16651, #2105, #8758 ) ;
#14908 = CARTESIAN_POINT ( 'NONE',  ( 8.904477399772744661, 142.4465447428235620, 19.33413753149157088 ) ) ;
#14909 = ADVANCED_FACE ( 'NONE', ( #17298 ), #17115, .F. ) ;
#14910 = AXIS2_PLACEMENT_3D ( 'NONE', #494, #8551, #16712 ) ;
#14911 = EDGE_LOOP ( 'NONE', ( #13432, #17429 ) ) ;
#14912 = CARTESIAN_POINT ( 'NONE',  ( 30.49999999999998224, 9.999999999999998224, 10.00000000000000178 ) ) ;
#14913 = CARTESIAN_POINT ( 'NONE',  ( -38.00000000000000000, 2.000000000000000000, -28.00000000000000355 ) ) ;
#14914 = LINE ( 'NONE', #2703, #15529 ) ;
#14915 = DIRECTION ( 'NONE',  ( -1.000000000000000000, -0.000000000000000000, 0.000000000000000000 ) ) ;
#14916 = FACE_BOUND ( 'NONE', #14697, .T. ) ;
#14917 = PRODUCT_DEFINITION_SHAPE ( 'NONE', 'NONE',  #1351 ) ;
#14918 = EDGE_LOOP ( 'NONE', ( #4271, #7092 ) ) ;
#14919 = CARTESIAN_POINT ( 'NONE',  ( 48.00000000000000711, 191.6227766016837677, 5.571800142134975431 ) ) ;
#14920 = AXIS2_PLACEMENT_3D ( 'NONE', #10051, #508, #7485 ) ;
#14921 = DIRECTION ( 'NONE',  ( -0.000000000000000000, 0.000000000000000000, -1.000000000000000000 ) ) ;
#14922 = CARTESIAN_POINT ( 'NONE',  ( 29.98123639043839006, 19.99999999999999645, -18.19121573219640098 ) ) ;
#14923 = CARTESIAN_POINT ( 'NONE',  ( 24.93507336697364707, 29.86842105263157876, 15.00000000000000000 ) ) ;
#14924 = CARTESIAN_POINT ( 'NONE',  ( -50.00000000000000000, 171.6227766016838245, 20.00000000000000355 ) ) ;
#14925 = AXIS2_PLACEMENT_3D ( 'NONE', #7475, #11198, #593 ) ;
#14926 = ORIENTED_EDGE ( 'NONE', *, *, #15904, .F. ) ;
#14927 = EDGE_CURVE ( 'NONE', #5676, #13633, #3377, .T. ) ;
#14928 = DIRECTION ( 'NONE',  ( -0.000000000000000000, -1.000000000000000000, 0.000000000000000000 ) ) ;
#14929 = VERTEX_POINT ( 'NONE', #2333 ) ;
#14930 = CARTESIAN_POINT ( 'NONE',  ( -70.00000000000000000, 204.6227766016838245, -2.020667218593133100E-15 ) ) ;
#14931 = VERTEX_POINT ( 'NONE', #6402 ) ;
#14932 = CIRCLE ( 'NONE', #3342, 20.00000000000000355 ) ;
#14933 = CARTESIAN_POINT ( 'NONE',  ( 17.00000000000000000, 171.6227766016838245, 0.000000000000000000 ) ) ;
#14934 = FACE_OUTER_BOUND ( 'NONE', #4949, .T. ) ;
#14935 = DIRECTION ( 'NONE',  ( 0.000000000000000000, 1.224646799147353207E-16, -1.000000000000000000 ) ) ;
#14936 = VERTEX_POINT ( 'NONE', #3576 ) ;
#14937 = DIRECTION ( 'NONE',  ( 0.000000000000000000, 0.000000000000000000, 1.000000000000000000 ) ) ;
#14938 = DIRECTION ( 'NONE',  ( 1.000000000000000000, -0.000000000000000000, -0.000000000000000000 ) ) ;
#14939 = DIRECTION ( 'NONE',  ( -0.000000000000000000, -0.000000000000000000, -1.000000000000000000 ) ) ;
#14940 = VECTOR ( 'NONE', #2313, 1000.000000000000000 ) ;
#14941 = EDGE_CURVE ( 'NONE', #15663, #12567, #8651, .T. ) ;
#14942 = AXIS2_PLACEMENT_3D ( 'NONE', #6011, #12912, #16899 ) ;
#14943 = PLANE ( 'NONE',  #6996 ) ;
#14944 = ORIENTED_EDGE ( 'NONE', *, *, #10791, .F. ) ;
#14945 = FACE_BOUND ( 'NONE', #10216, .T. ) ;
#14946 = PLANE ( 'NONE',  #3274 ) ;
#14947 = VERTEX_POINT ( 'NONE', #1455 ) ;
#14948 = CARTESIAN_POINT ( 'NONE',  ( -84.31671119272000681, 192.4368082929522075, -28.14105258436205403 ) ) ;
#14949 = AXIS2_PLACEMENT_3D ( 'NONE', #15908, #12996, #6616 ) ;
#14950 = EDGE_CURVE ( 'NONE', #5744, #12793, #1528, .T. ) ;
#14951 = EDGE_CURVE ( 'NONE', #6665, #11003, #4196, .T. ) ;
#14952 = CARTESIAN_POINT ( 'NONE',  ( -20.49999999999998224, 10.00000000000000000, -35.00200000000000244 ) ) ;
#14953 = AXIS2_PLACEMENT_3D ( 'NONE', #10804, #16214, #4080 ) ;
#14954 = AXIS2_PLACEMENT_3D ( 'NONE', #11191, #11456, #484 ) ;
#14955 = CARTESIAN_POINT ( 'NONE',  ( 31.90657348432143792, 191.9854139975491023, 25.96938468333276973 ) ) ;
#14956 = AXIS2_PLACEMENT_3D ( 'NONE', #12980, #15548, #8645 ) ;
#14957 = FACE_OUTER_BOUND ( 'NONE', #5393, .T. ) ;
#14958 = DIRECTION ( 'NONE',  ( 0.000000000000000000, 0.000000000000000000, 1.000000000000000000 ) ) ;
#14959 = CARTESIAN_POINT ( 'NONE',  ( -3.000000000000000888, 171.6227766016838245, 20.00000000000000355 ) ) ;
#14960 = CARTESIAN_POINT ( 'NONE',  ( 196.0000000000000000, 191.6227766016837677, -3.071800142134975431 ) ) ;
#14961 = SURFACE_STYLE_FILL_AREA ( #16298 ) ;
#14962 = EDGE_LOOP ( 'NONE', ( #14337, #17167, #10940, #13213 ) ) ;
#14963 = CARTESIAN_POINT ( 'NONE',  ( 196.0000000000000000, 155.6227766016839098, -10.00000337241049309 ) ) ;
#14964 = ORIENTED_EDGE ( 'NONE', *, *, #13788, .F. ) ;
#14965 = LINE ( 'NONE', #17, #9594 ) ;
#14966 = AXIS2_PLACEMENT_3D ( 'NONE', #12547, #12205, #8479 ) ;
#14967 = DIRECTION ( 'NONE',  ( 0.000000000000000000, 0.000000000000000000, 1.000000000000000000 ) ) ;
#14968 = AXIS2_PLACEMENT_3D ( 'NONE', #5150, #6216, #10538 ) ;
#14969 = ORIENTED_EDGE ( 'NONE', *, *, #4304, .F. ) ;
#14970 = CARTESIAN_POINT ( 'NONE',  ( -17.68452897573239824, 32.19524659542067013, 8.268362122121875046 ) ) ;
#14971 = AXIS2_PLACEMENT_3D ( 'NONE', #12763, #8774, #15499 ) ;
#14972 = DIRECTION ( 'NONE',  ( 1.000000000000000000, 0.000000000000000000, 0.000000000000000000 ) ) ;
#14973 = EDGE_LOOP ( 'NONE', ( #9237, #12545 ) ) ;
#14974 = CARTESIAN_POINT ( 'NONE',  ( 23.64306072442660422, 150.6299487802827741, -25.46745035168473237 ) ) ;
#14975 = ORIENTED_EDGE ( 'NONE', *, *, #155, .F. ) ;
#14976 = CARTESIAN_POINT ( 'NONE',  ( 39.99999999999998579, -20.00000000000000000, 39.99999999999998579 ) ) ;
#14977 = DIRECTION ( 'NONE',  ( 0.000000000000000000, -1.000000000000000000, 0.000000000000000000 ) ) ;
#14978 = CIRCLE ( 'NONE', #7352, 24.99999999999999645 ) ;
#14979 = DIRECTION ( 'NONE',  ( -1.000000000000000000, 0.000000000000000000, 0.000000000000000000 ) ) ;
#14980 = EDGE_LOOP ( 'NONE', ( #4737, #14553, #13993, #1442 ) ) ;
#14981 = DIRECTION ( 'NONE',  ( 1.000000000000000000, 0.000000000000000000, -0.000000000000000000 ) ) ;
#14982 = TOROIDAL_SURFACE ( 'NONE', #8770, 240.0000000000000000, 8.000000000000000000 ) ;
#14983 = ORIENTED_EDGE ( 'NONE', *, *, #13790, .F. ) ;
#14984 = CARTESIAN_POINT ( 'NONE',  ( 34.31805984300264356, 149.1480937705749170, 24.16447509748838840 ) ) ;
#14985 = EDGE_CURVE ( 'NONE', #13756, #3929, #13666, .T. ) ;
#14986 = ORIENTED_EDGE ( 'NONE', *, *, #15532, .T. ) ;
#14987 = CARTESIAN_POINT ( 'NONE',  ( 37.99999999999999289, 18.00000000000000355, 8.789265611615818404E-15 ) ) ;
#14988 = CARTESIAN_POINT ( 'NONE',  ( -80.00000000000001421, 196.6227766016838245, 0.000000000000000000 ) ) ;
#14989 = CARTESIAN_POINT ( 'NONE',  ( -16.22141882056480355, 32.74469488918423821, -6.141726134091478606 ) ) ;
#14990 = ORIENTED_EDGE ( 'NONE', *, *, #5157, .T. ) ;
#14991 = EDGE_LOOP ( 'NONE', ( #14422, #642, #12749, #9356 ) ) ;
#14992 = CIRCLE ( 'NONE', #5099, 2.500000000000002220 ) ;
#14993 = CIRCLE ( 'NONE', #16704, 2.499999999999998668 ) ;
#14994 = CARTESIAN_POINT ( 'NONE',  ( -195.2299705378136991, 174.0696332146309544, -3.384031243670033273 ) ) ;
#14995 = CARTESIAN_POINT ( 'NONE',  ( 49.99999999999998579, 167.6227766016838530, 5.571800142134975431 ) ) ;
#14996 = CIRCLE ( 'NONE', #14717, 10.00000000000000000 ) ;
#14997 = ORIENTED_EDGE ( 'NONE', *, *, #7355, .F. ) ;
#14998 = CYLINDRICAL_SURFACE ( 'NONE', #9349, 19.49999999999998934 ) ;
#14999 = CYLINDRICAL_SURFACE ( 'NONE', #2425, 7.500000000000020428 ) ;
#15000 = CARTESIAN_POINT ( 'NONE',  ( 18.47699279854304777, 29.92902263789611439, -12.17729482734268132 ) ) ;
#15001 = DIRECTION ( 'NONE',  ( 1.000000000000000000, 0.000000000000000000, 0.000000000000000000 ) ) ;
#15002 = CARTESIAN_POINT ( 'NONE',  ( 48.00000000000000711, 187.6227766016837961, -15.00000337241049486 ) ) ;
#15003 = EDGE_LOOP ( 'NONE', ( #7845, #8875, #7832, #15261 ) ) ;
#15004 = CARTESIAN_POINT ( 'NONE',  ( -76.52069396612810692, 201.5149201033276256, -18.20725769141078487 ) ) ;
#15005 = AXIS2_PLACEMENT_3D ( 'NONE', #12353, #11373, #11022 ) ;
#15006 = EDGE_CURVE ( 'NONE', #9729, #9167, #10907, .T. ) ;
#15007 = ADVANCED_FACE ( 'NONE', ( #4032 ), #13269, .F. ) ;
#15008 = DIRECTION ( 'NONE',  ( 0.000000000000000000, 0.000000000000000000, 1.000000000000000000 ) ) ;
#15009 = EDGE_CURVE ( 'NONE', #2789, #10402, #14392, .T. ) ;
#15010 = DIRECTION ( 'NONE',  ( -2.312964634635742464E-16, 0.000000000000000000, -1.000000000000000000 ) ) ;
#15011 = CARTESIAN_POINT ( 'NONE',  ( -43.00000000000000711, 130.0000000000000000, -12.99999999999999822 ) ) ;
#15012 = DIRECTION ( 'NONE',  ( -1.000000000000000000, 0.000000000000000000, 0.000000000000000000 ) ) ;
#15013 = VERTEX_POINT ( 'NONE', #17479 ) ;
#15014 = LINE ( 'NONE', #6875, #10176 ) ;
#15015 = ORIENTED_EDGE ( 'NONE', *, *, #17384, .T. ) ;
#15016 = FACE_OUTER_BOUND ( 'NONE', #1792, .T. ) ;
#15017 = VECTOR ( 'NONE', #2603, 1000.000000000000000 ) ;
#15018 = ORIENTED_EDGE ( 'NONE', *, *, #5815, .F. ) ;
#15019 = CARTESIAN_POINT ( 'NONE',  ( -40.00000000000000000, 4.000000000000000000, -30.00000000000000000 ) ) ;
#15020 = DIRECTION ( 'NONE',  ( 0.000000000000000000, 0.000000000000000000, 1.000000000000000000 ) ) ;
#15021 = CARTESIAN_POINT ( 'NONE',  ( 39.99999999999998579, 0.000000000000000000, 33.00000000000001421 ) ) ;
#15022 = VERTEX_POINT ( 'NONE', #2689 ) ;
#15023 = LINE ( 'NONE', #6882, #8407 ) ;
#15024 = DIRECTION ( 'NONE',  ( 1.000000000000000000, 0.000000000000000000, -0.000000000000000000 ) ) ;
#15025 = CARTESIAN_POINT ( 'NONE',  ( 0.000000000000000000, 18.00000000000000355, 0.000000000000000000 ) ) ;
#15026 = LINE ( 'NONE', #13805, #12872 ) ;
#15027 = CARTESIAN_POINT ( 'NONE',  ( 17.42040306417330342, 125.8667821340875577, -6.358709916038607801 ) ) ;
#15028 = ORIENTED_EDGE ( 'NONE', *, *, #6133, .F. ) ;
#15029 = DIRECTION ( 'NONE',  ( 1.000000000000000000, 0.000000000000000000, 0.000000000000000000 ) ) ;
#15030 = DIRECTION ( 'NONE',  ( 1.000000000000000000, 0.000000000000000000, 0.000000000000000000 ) ) ;
#15031 = ORIENTED_EDGE ( 'NONE', *, *, #6577, .T. ) ;
#15032 = CARTESIAN_POINT ( 'NONE',  ( -74.95488020859191636, 193.3541989604593425, -27.43934207688683813 ) ) ;
#15033 = CYLINDRICAL_SURFACE ( 'NONE', #5325, 7.500000000000007105 ) ;
#15034 = EDGE_CURVE ( 'NONE', #3748, #1902, #2281, .T. ) ;
#15035 = LINE ( 'NONE', #263, #17149 ) ;
#15036 = EDGE_CURVE ( 'NONE', #5017, #2637, #6769, .T. ) ;
#15037 = CARTESIAN_POINT ( 'NONE',  ( 34.26588824652853305, 18.00000000000000000, -10.16858984204336736 ) ) ;
#15038 = DIRECTION ( 'NONE',  ( -1.000000000000000000, 0.000000000000000000, 0.000000000000000000 ) ) ;
#15039 = CARTESIAN_POINT ( 'NONE',  ( 196.0000000000000000, 167.6227766016838530, -5.571800142134975431 ) ) ;
#15040 = DIRECTION ( 'NONE',  ( 0.9961946980917461003, 0.000000000000000000, -0.08715574274765162943 ) ) ;
#15041 = CARTESIAN_POINT ( 'NONE',  ( -85.00000000000002842, 146.6227766016838245, 0.000000000000000000 ) ) ;
#15042 = VERTEX_POINT ( 'NONE', #11354 ) ;
#15043 = CARTESIAN_POINT ( 'NONE',  ( -25.16839285024614625, 19.99999999999999645, -15.12082343620048519 ) ) ;
#15044 = ORIENTED_EDGE ( 'NONE', *, *, #5544, .T. ) ;
#15045 = DIRECTION ( 'NONE',  ( -1.000000000000000000, 0.000000000000000000, 0.000000000000000000 ) ) ;
#15046 = ADVANCED_FACE ( 'NONE', ( #11260 ), #7023, .F. ) ;
#15047 = DIRECTION ( 'NONE',  ( 0.000000000000000000, 0.000000000000000000, 1.000000000000000000 ) ) ;
#15048 = ORIENTED_EDGE ( 'NONE', *, *, #5218, .F. ) ;
#15049 = CARTESIAN_POINT ( 'NONE',  ( -17.27091434876127707, 32.11264161353675917, 9.179609695281474302 ) ) ;
#15050 = DIRECTION ( 'NONE',  ( -0.000000000000000000, -0.000000000000000000, 1.000000000000000000 ) ) ;
#15051 = VERTEX_POINT ( 'NONE', #15419 ) ;
#15052 = PRODUCT_DEFINITION_SHAPE ( 'NONE', 'NONE',  #17531 ) ;
#15053 = CARTESIAN_POINT ( 'NONE',  ( 36.08081429761088543, 151.0194919042433241, -25.77925661938085611 ) ) ;
#15054 = ORIENTED_EDGE ( 'NONE', *, *, #7681, .T. ) ;
#15055 = EDGE_CURVE ( 'NONE', #11435, #7753, #4459, .T. ) ;
#15056 = CARTESIAN_POINT ( 'NONE',  ( 35.45515645957151918, 191.4518784269448588, -26.38258506112510560 ) ) ;
#15057 = CARTESIAN_POINT ( 'NONE',  ( 196.0000000000000000, 175.6227766016838245, -8.071800142134975431 ) ) ;
#15058 = ORIENTED_EDGE ( 'NONE', *, *, #5249, .T. ) ;
#15059 = CARTESIAN_POINT ( 'NONE',  ( 27.44407568426044008, 138.8271129316868837, 3.666666666666658081 ) ) ;
#15060 = CARTESIAN_POINT ( 'NONE',  ( -24.99999999999999289, 90.00000000000000000, -15.00000000000000000 ) ) ;
#15061 = ORIENTED_EDGE ( 'NONE', *, *, #8585, .T. ) ;
#15062 = DIRECTION ( 'NONE',  ( 0.000000000000000000, 0.000000000000000000, -1.000000000000000000 ) ) ;
#15063 = EDGE_CURVE ( 'NONE', #15578, #14384, #4716, .T. ) ;
#15064 = ORIENTED_EDGE ( 'NONE', *, *, #17303, .F. ) ;
#15065 = EDGE_CURVE ( 'NONE', #12692, #17091, #15161, .T. ) ;
#15066 = DIRECTION ( 'NONE',  ( 1.000000000000000000, 0.000000000000000000, -0.000000000000000000 ) ) ;
#15067 = DIRECTION ( 'NONE',  ( -1.000000000000000000, -0.000000000000000000, 0.000000000000000000 ) ) ;
#15068 = ADVANCED_FACE ( 'NONE', ( #12590 ), #4549, .F. ) ;
#15069 = FACE_OUTER_BOUND ( 'NONE', #9670, .T. ) ;
#15070 = ORIENTED_EDGE ( 'NONE', *, *, #6679, .T. ) ;
#15071 = ORIENTED_EDGE ( 'NONE', *, *, #12023, .T. ) ;
#15072 = DIRECTION ( 'NONE',  ( 0.000000000000000000, 0.000000000000000000, -1.000000000000000000 ) ) ;
#15073 = CARTESIAN_POINT ( 'NONE',  ( 17.58250999373982282, 125.2198453306090045, 5.979920648958140776E-13 ) ) ;
#15074 = CARTESIAN_POINT ( 'NONE',  ( 8.608950980928550933, 133.4921716645119432, 14.72901497434506091 ) ) ;
#15075 = VERTEX_POINT ( 'NONE', #8432 ) ;
#15076 = PRODUCT_CONTEXT ( 'NONE', #15236, 'mechanical' ) ;
#15077 = EDGE_CURVE ( 'NONE', #14256, #11533, #13931, .T. ) ;
#15078 = CYLINDRICAL_SURFACE ( 'NONE', #12050, 7.500000000000000000 ) ;
#15079 = CARTESIAN_POINT ( 'NONE',  ( 22.73104287435775461, 29.84603067649059227, -6.814483377121257845 ) ) ;
#15080 = LINE ( 'NONE', #8618, #13899 ) ;
#15081 = CARTESIAN_POINT ( 'NONE',  ( 15.97577464858015617, 18.00000000000457234, 12.97048270532338243 ) ) ;
#15082 = VERTEX_POINT ( 'NONE', #9846 ) ;
#15083 = DIRECTION ( 'NONE',  ( -0.000000000000000000, -0.000000000000000000, -1.000000000000000000 ) ) ;
#15084 = CYLINDRICAL_SURFACE ( 'NONE', #3989, 19.49999999999999645 ) ;
#15085 = DIRECTION ( 'NONE',  ( 0.000000000000000000, 0.000000000000000000, -1.000000000000000000 ) ) ;
#15086 = CARTESIAN_POINT ( 'NONE',  ( -208.1243153690002430, 172.6001711966515018, 5.795976030063606288 ) ) ;
#15087 = LINE ( 'NONE', #3056, #9503 ) ;
#15088 = UNCERTAINTY_MEASURE_WITH_UNIT (LENGTH_MEASURE( 1.000000000000000082E-05 ), #17488, 'distance_accuracy_value', 'NONE');
#15089 = ORIENTED_EDGE ( 'NONE', *, *, #11203, .T. ) ;
#15090 = VERTEX_POINT ( 'NONE', #12775 ) ;
#15091 = DIRECTION ( 'NONE',  ( 1.000000000000000000, -0.000000000000000000, -0.000000000000000000 ) ) ;
#15092 = VERTEX_POINT ( 'NONE', #15251 ) ;
#15093 = VERTEX_POINT ( 'NONE', #16681 ) ;
#15094 = EDGE_CURVE ( 'NONE', #4421, #2973, #13753, .T. ) ;
#15095 = EDGE_CURVE ( 'NONE', #13912, #10145, #1972, .T. ) ;
#15096 = CARTESIAN_POINT ( 'NONE',  ( -48.00000000000000000, 171.6227766016838245, 0.000000000000000000 ) ) ;
#15097 = EDGE_CURVE ( 'NONE', #13521, #3793, #4632, .T. ) ;
#15098 = FACE_BOUND ( 'NONE', #2807, .T. ) ;
#15099 = CIRCLE ( 'NONE', #7468, 2.499999999999998668 ) ;
#15100 = CARTESIAN_POINT ( 'NONE',  ( -206.3689767832464668, 166.7044760491588988, 0.5444864983987496299 ) ) ;
#15101 = DIRECTION ( 'NONE',  ( -1.000000000000000000, -0.000000000000000000, -0.000000000000000000 ) ) ;
#15102 = ORIENTED_EDGE ( 'NONE', *, *, #5920, .F. ) ;
#15103 = CARTESIAN_POINT ( 'NONE',  ( -5.000000000000004441, 144.1839557653416080, 18.33333333333336057 ) ) ;
#15104 = FACE_OUTER_BOUND ( 'NONE', #1658, .T. ) ;
#15105 = FACE_BOUND ( 'NONE', #17256, .T. ) ;
#15106 = CARTESIAN_POINT ( 'NONE',  ( -155.0000000000000284, 171.6227766016838245, 0.000000000000000000 ) ) ;
#15107 = VECTOR ( 'NONE', #2050, 1000.000000000000000 ) ;
#15108 = VECTOR ( 'NONE', #15180, 1000.000000000000000 ) ;
#15109 = LINE ( 'NONE', #9537, #11248 ) ;
#15110 = ORIENTED_EDGE ( 'NONE', *, *, #4029, .F. ) ;
#15111 = FACE_BOUND ( 'NONE', #14579, .T. ) ;
#15112 = DIRECTION ( 'NONE',  ( 1.000000000000000000, 0.000000000000000000, 1.445602896647339163E-16 ) ) ;
#15113 = ORIENTED_EDGE ( 'NONE', *, *, #5788, .T. ) ;
#15114 = EDGE_CURVE ( 'NONE', #2291, #13060, #16093, .T. ) ;
#15115 = DIRECTION ( 'NONE',  ( 0.000000000000000000, 0.000000000000000000, 1.000000000000000000 ) ) ;
#15116 = DIRECTION ( 'NONE',  ( 0.000000000000000000, 0.000000000000000000, 1.000000000000000000 ) ) ;
#15117 =( REPRESENTATION_RELATIONSHIP ('NONE','NONE', #9723, #6585 ) REPRESENTATION_RELATIONSHIP_WITH_TRANSFORMATION ( #3218 )SHAPE_REPRESENTATION_RELATIONSHIP( ) );
#15118 = LINE ( 'NONE', #2831, #16597 ) ;
#15119 = CARTESIAN_POINT ( 'NONE',  ( -25.49999999999998579, 10.00000000000000000, 0.000000000000000000 ) ) ;
#15120 = AXIS2_PLACEMENT_3D ( 'NONE', #12843, #3289, #12767 ) ;
#15121 = CARTESIAN_POINT ( 'NONE',  ( -32.64269715136552463, 118.7804878048780779, 5.500000000000000000 ) ) ;
#15122 = CARTESIAN_POINT ( 'NONE',  ( 14.93242934743710393, 30.00000000000000000, 13.00000000000000178 ) ) ;
#15123 = COLOUR_RGB ( '', 0.66274510, 0.83137255, 0.94901961) ;
#15124 = CARTESIAN_POINT ( 'NONE',  ( -77.32133379281293628, 200.8588467739806163, 15.30956876290917457 ) ) ;
#15125 = VECTOR ( 'NONE', #3244, 1000.000000000000000 ) ;
#15126 = DIRECTION ( 'NONE',  ( -0.000000000000000000, -0.000000000000000000, -1.000000000000000000 ) ) ;
#15127 = ORIENTED_EDGE ( 'NONE', *, *, #9480, .F. ) ;
#15128 = ORIENTED_EDGE ( 'NONE', *, *, #2696, .F. ) ;
#15129 = CARTESIAN_POINT ( 'NONE',  ( 22.87244304995705235, 29.89498257257996272, -11.09085247437311494 ) ) ;
#15130 = DIRECTION ( 'NONE',  ( 0.000000000000000000, 0.000000000000000000, -1.000000000000000000 ) ) ;
#15131 = VERTEX_POINT ( 'NONE', #560 ) ;
#15132 = ADVANCED_FACE ( 'NONE', ( #1716 ), #1625, .F. ) ;
#15133 = CARTESIAN_POINT ( 'NONE',  ( -15.98664213571245440, 31.85373729401663212, 11.16351695777366082 ) ) ;
#15134 = FACE_OUTER_BOUND ( 'NONE', #13382, .T. ) ;
#15135 = COLOUR_RGB ( '', 0.66274510, 0.83137255, 0.94901961) ;
#15136 = VERTEX_POINT ( 'NONE', #375 ) ;
#15137 = AXIS2_PLACEMENT_3D ( 'NONE', #12640, #7070, #5915 ) ;
#15138 = CARTESIAN_POINT ( 'NONE',  ( 22.50000000000002132, 146.8102797458443831, -21.75827460206394903 ) ) ;
#15139 = AXIS2_PLACEMENT_3D ( 'NONE', #11341, #10182, #14182 ) ;
#15140 = DIRECTION ( 'NONE',  ( -1.000000000000000000, 0.000000000000000000, 0.000000000000000000 ) ) ;
#15141 = CYLINDRICAL_SURFACE ( 'NONE', #15733, 2.500000000000000444 ) ;
#15142 = FACE_BOUND ( 'NONE', #7088, .T. ) ;
#15143 = LINE ( 'NONE', #3022, #6840 ) ;
#15144 = DIRECTION ( 'NONE',  ( 1.000000000000000000, 0.000000000000000000, 0.000000000000000000 ) ) ;
#15145 = B_SPLINE_CURVE_WITH_KNOTS ( 'NONE', 3,
 ( #5937, #13989, #4431, #6899, #12656, #8496, #15312, #10970, #8305, #1592, #16652, #11061, #266, #5672, #4519, #3185, #9725, #9552, #13640, #8402, #1852, #172, #15122 ),
 .UNSPECIFIED., .F., .F.,
 ( 4, 2, 2, 2, 2, 2, 2, 2, 1, 2, 2, 4 ),
 ( 0.000000000000000000, 0.001562580732212274365, 0.002343871098318411547, 0.003125161464424548730, 0.004687742196636830901, 0.006250322928849113939, 0.007812903661061397845, 0.008594194027167533292, 0.009375484393273670475, 0.01015677475937980939, 0.01093806512548594484, 0.01250064585769823135 ),
 .UNSPECIFIED. ) ;
#15146 = DIRECTION ( 'NONE',  ( -0.000000000000000000, -0.000000000000000000, -1.000000000000000000 ) ) ;
#15147 = CIRCLE ( 'NONE', #17420, 23.57392898041429774 ) ;
#15148 = VERTEX_POINT ( 'NONE', #5775 ) ;
#15149 = CARTESIAN_POINT ( 'NONE',  ( -100.0000000000000000, 171.6227766016838245, 0.000000000000000000 ) ) ;
#15150 = AXIS2_PLACEMENT_3D ( 'NONE', #9755, #16331, #5520 ) ;
#15151 = ORIENTED_EDGE ( 'NONE', *, *, #7317, .T. ) ;
#15152 = CARTESIAN_POINT ( 'NONE',  ( -72.65335638526123319, 195.0609035571773404, -23.23759988234784046 ) ) ;
#15153 = CARTESIAN_POINT ( 'NONE',  ( -48.00000000000000000, 171.6227766016838245, -20.00000000000000355 ) ) ;
#15154 = DIRECTION ( 'NONE',  ( -0.000000000000000000, -0.000000000000000000, -1.000000000000000000 ) ) ;
#15155 = CIRCLE ( 'NONE', #12334, 12.00000000000000000 ) ;
#15156 = ORIENTED_EDGE ( 'NONE', *, *, #1703, .T. ) ;
#15157 = EDGE_LOOP ( 'NONE', ( #9189, #1531 ) ) ;
#15158 = ADVANCED_FACE ( 'NONE', ( #7189 ), #4365, .T. ) ;
#15159 = LINE ( 'NONE', #3036, #7470 ) ;
#15160 = DIRECTION ( 'NONE',  ( -1.000000000000000000, -0.000000000000000000, -0.000000000000000000 ) ) ;
#15161 = B_SPLINE_CURVE_WITH_KNOTS ( 'NONE', 3,
 ( #7108, #8523, #14015, #1885 ),
 .UNSPECIFIED., .F., .F.,
 ( 4, 4 ),
 ( 0.000000000000000000, 0.003888888888888887042 ),
 .UNSPECIFIED. ) ;
#15162 = CARTESIAN_POINT ( 'NONE',  ( 17.52204077229825785, 125.6458339596819798, 5.684362142990314837 ) ) ;
#15163 = VECTOR ( 'NONE', #13996, 1000.000000000000000 ) ;
#15164 = CIRCLE ( 'NONE', #16305, 2.500000000000000000 ) ;
#15165 = PRODUCT_RELATED_PRODUCT_CATEGORY ( 'part', '', ( #7438 ) ) ;
#15166 = ORIENTED_EDGE ( 'NONE', *, *, #6963, .T. ) ;
#15167 = DIRECTION ( 'NONE',  ( -0.000000000000000000, -0.000000000000000000, 1.000000000000000000 ) ) ;
#15168 = AXIS2_PLACEMENT_3D ( 'NONE', #11368, #2958, #14033 ) ;
#15169 = EDGE_CURVE ( 'NONE', #6472, #13341, #10727, .T. ) ;
#15170 = CARTESIAN_POINT ( 'NONE',  ( -31.66708739526795924, 100.0000000000000142, 5.500000000000000000 ) ) ;
#15171 = EDGE_CURVE ( 'NONE', #16623, #6275, #8181, .T. ) ;
#15172 = AXIS2_PLACEMENT_3D ( 'NONE', #8486, #13809, #16379 ) ;
#15173 = DIRECTION ( 'NONE',  ( 1.000000000000000000, 0.000000000000000000, 0.000000000000000000 ) ) ;
#15174 = CARTESIAN_POINT ( 'NONE',  ( 48.00000000000000711, 175.6227766016838530, -16.92820660268601429 ) ) ;
#15175 = CARTESIAN_POINT ( 'NONE',  ( 20.11141720500412333, 18.00000000000000000, 24.32074799214299077 ) ) ;
#15176 = LINE ( 'NONE', #1731, #16243 ) ;
#15177 = VERTEX_POINT ( 'NONE', #4966 ) ;
#15178 = CARTESIAN_POINT ( 'NONE',  ( -74.65276356201289332, 199.3666727680385975, -21.34312735376092718 ) ) ;
#15179 = PLANE ( 'NONE',  #7643 ) ;
#15180 = DIRECTION ( 'NONE',  ( 0.000000000000000000, 0.000000000000000000, 1.000000000000000000 ) ) ;
#15181 = CARTESIAN_POINT ( 'NONE',  ( 32.99999999999998579, 9.999999999999998224, 35.00200000000000244 ) ) ;
#15182 = DIRECTION ( 'NONE',  ( 0.000000000000000000, 0.000000000000000000, 1.000000000000000000 ) ) ;
#15183 = ORIENTED_EDGE ( 'NONE', *, *, #9928, .F. ) ;
#15184 = AXIS2_PLACEMENT_3D ( 'NONE', #12655, #7252, #7345 ) ;
#15185 = ORIENTED_EDGE ( 'NONE', *, *, #17287, .F. ) ;
#15186 = COLOUR_RGB ( '', 0.40784314, 0.44705882, 0.49803922) ;
#15187 = DIRECTION ( 'NONE',  ( -0.000000000000000000, -0.000000000000000000, -1.000000000000000000 ) ) ;
#15188 = ORIENTED_EDGE ( 'NONE', *, *, #847, .T. ) ;
#15189 = CARTESIAN_POINT ( 'NONE',  ( -195.2299705378136423, 167.4686912709917408, -0.4270243643951285861 ) ) ;
#15190 = ORIENTED_EDGE ( 'NONE', *, *, #9422, .F. ) ;
#15191 = CARTESIAN_POINT ( 'NONE',  ( -45.00000000000000000, 120.0000000000000142, 0.000000000000000000 ) ) ;
#15192 = LINE ( 'NONE', #2893, #2138 ) ;
#15193 = DIRECTION ( 'NONE',  ( -1.000000000000000000, 0.000000000000000000, 0.000000000000000000 ) ) ;
#15194 = CARTESIAN_POINT ( 'NONE',  ( -68.00000000000000000, 154.3022685259950038, -9.999999999999900524 ) ) ;
#15195 = AXIS2_PLACEMENT_3D ( 'NONE', #1832, #15464, #12811 ) ;
#15196 = PRODUCT_DEFINITION_FORMATION_WITH_SPECIFIED_SOURCE ( 'ANY', '', #3197, .NOT_KNOWN. ) ;
#15197 = CARTESIAN_POINT ( 'NONE',  ( 21.87797949700605926, 29.86248177612424115, -9.008363892349379398 ) ) ;
#15198 = AXIS2_PLACEMENT_3D ( 'NONE', #5619, #14818, #9414 ) ;
#15199 = EDGE_LOOP ( 'NONE', ( #15541, #6652, #12242, #11781 ) ) ;
#15200 = CARTESIAN_POINT ( 'NONE',  ( -167.6513770290094385, 170.3104757200652273, 2.272971801780875989 ) ) ;
#15201 = DIRECTION ( 'NONE',  ( 0.000000000000000000, 0.000000000000000000, -1.000000000000000000 ) ) ;
#15202 = DIRECTION ( 'NONE',  ( -1.000000000000000000, -0.000000000000000000, -0.000000000000000000 ) ) ;
#15203 = DIRECTION ( 'NONE',  ( 0.000000000000000000, 0.000000000000000000, -1.000000000000000000 ) ) ;
#15204 = EDGE_CURVE ( 'NONE', #8060, #5440, #2225, .T. ) ;
#15205 = PRODUCT ( 'BR-801', 'BR-801', '', ( #8909 ) ) ;
#15206 = CARTESIAN_POINT ( 'NONE',  ( -31.66708739526795924, 119.0000000000000284, 5.500000000000000000 ) ) ;
#15207 = AXIS2_PLACEMENT_3D ( 'NONE', #11816, #13150, #8897 ) ;
#15208 = EDGE_LOOP ( 'NONE', ( #8546, #2995, #11956, #11691, #3525, #710 ) ) ;
#15209 = CARTESIAN_POINT ( 'NONE',  ( -68.00000000000000000, 171.6227766016838245, 24.99999999999999289 ) ) ;
#15210 = VECTOR ( 'NONE', #9381, 1000.000000000000000 ) ;
#15211 = PRESENTATION_LAYER_ASSIGNMENT (  '', '', ( #1372 ) ) ;
#15212 = ORIENTED_EDGE ( 'NONE', *, *, #7428, .T. ) ;
#15213 = SURFACE_SIDE_STYLE ('',( #4510 ) ) ;
#15214 = CARTESIAN_POINT ( 'NONE',  ( -74.38629067462862565, 194.4974200864254215, -26.49149599578361247 ) ) ;
#15215 = DIRECTION ( 'NONE',  ( -1.000000000000000000, 0.000000000000000000, 0.000000000000000000 ) ) ;
#15216 = CARTESIAN_POINT ( 'NONE',  ( 25.00000000000000000, 196.6227766016838245, 21.54065922853802562 ) ) ;
#15217 = DIRECTION ( 'NONE',  ( 0.000000000000000000, -1.000000000000000000, 0.000000000000000000 ) ) ;
#15218 = CARTESIAN_POINT ( 'NONE',  ( -208.0000000000000853, 170.0678595944000620, 2.693195258168412654 ) ) ;
#15219 = LINE ( 'NONE', #12392, #11555 ) ;
#15220 = AXIS2_PLACEMENT_3D ( 'NONE', #16763, #7186, #7106 ) ;
#15221 = DIRECTION ( 'NONE',  ( -1.000000000000000000, -0.000000000000000000, 0.000000000000000000 ) ) ;
#15222 = AXIS2_PLACEMENT_3D ( 'NONE', #951, #14583, #7853 ) ;
#15223 = ORIENTED_EDGE ( 'NONE', *, *, #5054, .F. ) ;
#15224 = EDGE_CURVE ( 'NONE', #15613, #8372, #7610, .T. ) ;
#15225 = ADVANCED_FACE ( 'NONE', ( #13114 ), #17186, .T. ) ;
#15226 = ADVANCED_FACE ( 'NONE', ( #820 ), #14449, .T. ) ;
#15227 = ORIENTED_EDGE ( 'NONE', *, *, #6071, .T. ) ;
#15228 = DIRECTION ( 'NONE',  ( -0.000000000000000000, -0.000000000000000000, -1.000000000000000000 ) ) ;
#15229 = ADVANCED_FACE ( 'NONE', ( #14268 ), #11612, .T. ) ;
#15230 = CARTESIAN_POINT ( 'NONE',  ( -48.00000000000000000, 171.6227766016838245, 0.000000000000000000 ) ) ;
#15231 = ORIENTED_EDGE ( 'NONE', *, *, #9584, .T. ) ;
#15232 = CARTESIAN_POINT ( 'NONE',  ( 39.99999999999998579, 4.000000000000000000, -30.00000000000000000 ) ) ;
#15233 = DIRECTION ( 'NONE',  ( 0.000000000000000000, 0.000000000000000000, 1.000000000000000000 ) ) ;
#15234 = AXIS2_PLACEMENT_3D ( 'NONE', #14424, #13090, #8916 ) ;
#15235 = ORIENTED_EDGE ( 'NONE', *, *, #9480, .T. ) ;
#15236 = APPLICATION_CONTEXT ( 'automotive_design' ) ;
#15237 = VECTOR ( 'NONE', #6675, 1000.000000000000114 ) ;
#15238 = CYLINDRICAL_SURFACE ( 'NONE', #1685, 2.499999999999998668 ) ;
#15239 = AXIS2_PLACEMENT_3D ( 'NONE', #4560, #4641, #3221 ) ;
#15240 = CYLINDRICAL_SURFACE ( 'NONE', #9345, 10.00000000000000178 ) ;
#15241 = DIRECTION ( 'NONE',  ( 1.000000000000000000, 0.000000000000000000, 0.000000000000000000 ) ) ;
#15242 = CARTESIAN_POINT ( 'NONE',  ( -85.00000000000002842, 196.6227766016838245, 0.000000000000000000 ) ) ;
#15243 = DIRECTION ( 'NONE',  ( 0.000000000000000000, 0.000000000000000000, 1.000000000000000000 ) ) ;
#15244 = CARTESIAN_POINT ( 'NONE',  ( -32.59761674097720174, 119.3792650757569191, 5.080178642862611227 ) ) ;
#15245 = ADVANCED_FACE ( 'NONE', ( #4805 ), #10272, .T. ) ;
#15246 = CARTESIAN_POINT ( 'NONE',  ( -23.00000000000000000, 120.0000000000000284, -15.00000000000000000 ) ) ;
#15247 = ORIENTED_EDGE ( 'NONE', *, *, #6100, .T. ) ;
#15248 = FACE_OUTER_BOUND ( 'NONE', #13892, .T. ) ;
#15249 = AXIS2_PLACEMENT_3D ( 'NONE', #12946, #7448, #8860 ) ;
#15250 = ORIENTED_EDGE ( 'NONE', *, *, #3532, .F. ) ;
#15251 = CARTESIAN_POINT ( 'NONE',  ( -187.6513770290095238, 172.4976050944027008, 4.898587196589412829E-16 ) ) ;
#15252 = CIRCLE ( 'NONE', #3093, 2.500000000000000444 ) ;
#15253 = CARTESIAN_POINT ( 'NONE',  ( 2.950000000000001066, 0.000000000000000000, 0.000000000000000000 ) ) ;
#15254 = EDGE_LOOP ( 'NONE', ( #11552, #6106, #708, #7133 ) ) ;
#15255 = VERTEX_POINT ( 'NONE', #10361 ) ;
#15256 = LINE ( 'NONE', #8609, #8311 ) ;
#15257 = CARTESIAN_POINT ( 'NONE',  ( -187.6513770290094669, 171.1853623553243722, -0.7576236986489900405 ) ) ;
#15258 = CARTESIAN_POINT ( 'NONE',  ( 15.14881438696876614, 128.6905335926829252, 10.89137921944116449 ) ) ;
#15259 = VECTOR ( 'NONE', #278, 1000.000000000000000 ) ;
#15260 = CIRCLE ( 'NONE', #4247, 2.500000000000002220 ) ;
#15261 = ORIENTED_EDGE ( 'NONE', *, *, #16199, .T. ) ;
#15262 = CARTESIAN_POINT ( 'NONE',  ( -38.00000000000000000, 18.00000000000000355, 0.000000000000000000 ) ) ;
#15263 = CIRCLE ( 'NONE', #5664, 12.00000000000001421 ) ;
#15264 = CARTESIAN_POINT ( 'NONE',  ( -80.00000000000002842, 146.6227766016838245, -16.00000000000000000 ) ) ;
#15265 = CARTESIAN_POINT ( 'NONE',  ( -84.91986817799207188, 195.5664139939901531, 22.72185355927995687 ) ) ;
#15266 = DIRECTION ( 'NONE',  ( -0.000000000000000000, -0.000000000000000000, -1.000000000000000000 ) ) ;
#15267 = EDGE_CURVE ( 'NONE', #16797, #15922, #2397, .T. ) ;
#15268 = CARTESIAN_POINT ( 'NONE',  ( 14.93242934743710570, 30.00000000000000000, 13.00000000000000178 ) ) ;
#15269 = CYLINDRICAL_SURFACE ( 'NONE', #13695, 2.500000000000000444 ) ;
#15270 = EDGE_CURVE ( 'NONE', #13341, #6472, #7341, .T. ) ;
#15271 = ORIENTED_EDGE ( 'NONE', *, *, #10444, .T. ) ;
#15272 = CARTESIAN_POINT ( 'NONE',  ( -74.00000000000002842, 196.9987679943318142, -24.11115281963768453 ) ) ;
#15273 = CARTESIAN_POINT ( 'NONE',  ( 25.49999999999998579, 9.999999999999998224, 1.387778780781445676E-14 ) ) ;
#15274 = DIRECTION ( 'NONE',  ( 0.000000000000000000, 0.000000000000000000, 1.000000000000000000 ) ) ;
#15275 = DIRECTION ( 'NONE',  ( 1.000000000000000000, 0.000000000000000000, 0.000000000000000000 ) ) ;
#15276 = CYLINDRICAL_SURFACE ( 'NONE', #12052, 2.500000000000002220 ) ;
#15277 = CIRCLE ( 'NONE', #6806, 2.500000000000000444 ) ;
#15278 = EDGE_LOOP ( 'NONE', ( #1948, #6056, #3896, #14456 ) ) ;
#15279 = EDGE_LOOP ( 'NONE', ( #14209, #15654 ) ) ;
#15280 = AXIS2_PLACEMENT_3D ( 'NONE', #13142, #17392, #6509 ) ;
#15281 = EDGE_CURVE ( 'NONE', #6709, #15643, #3952, .T. ) ;
#15282 = CARTESIAN_POINT ( 'NONE',  ( 13.85534145189780197, 143.5014890223674229, 17.26861023069377410 ) ) ;
#15283 = EDGE_LOOP ( 'NONE', ( #12537, #9140, #10108, #17275 ) ) ;
#15284 = CARTESIAN_POINT ( 'NONE',  ( -80.00000000000002842, 146.6227766016838245, -12.99999999999999822 ) ) ;
#15285 = ORIENTED_EDGE ( 'NONE', *, *, #1704, .T. ) ;
#15286 =( NAMED_UNIT ( * ) SI_UNIT ( $, .STERADIAN. ) SOLID_ANGLE_UNIT ( ) );
#15287 = LINE ( 'NONE', #15364, #5959 ) ;
#15288 = SURFACE_SIDE_STYLE ('',( #856 ) ) ;
#15289 = CARTESIAN_POINT ( 'NONE',  ( -45.00000000000000000, 134.2062027339443944, 15.00000000000000000 ) ) ;
#15290 = CIRCLE ( 'NONE', #9061, 7.500000000000003553 ) ;
#15291 = DIRECTION ( 'NONE',  ( 0.8660254037844378194, -0.5000000000000015543, -0.000000000000000000 ) ) ;
#15292 = CIRCLE ( 'NONE', #876, 8.000000000000000000 ) ;
#15293 = ORIENTED_EDGE ( 'NONE', *, *, #8283, .T. ) ;
#15294 = CARTESIAN_POINT ( 'NONE',  ( 26.35862406984590578, 143.1840127716920961, 16.74578779913501947 ) ) ;
#15295 = FACE_OUTER_BOUND ( 'NONE', #13941, .T. ) ;
#15296 = DIRECTION ( 'NONE',  ( -1.000000000000000000, 0.000000000000000000, 0.000000000000000000 ) ) ;
#15297 = DIRECTION ( 'NONE',  ( 1.000000000000000000, -0.000000000000000000, -0.000000000000000000 ) ) ;
#15298 = EDGE_CURVE ( 'NONE', #2717, #11143, #14406, .T. ) ;
#15299 = AXIS2_PLACEMENT_3D ( 'NONE', #4475, #15266, #5713 ) ;
#15300 = LINE ( 'NONE', #3351, #7630 ) ;
#15301 = ORIENTED_EDGE ( 'NONE', *, *, #5126, .T. ) ;
#15302 = DIRECTION ( 'NONE',  ( -0.000000000000000000, 0.000000000000000000, -1.000000000000000000 ) ) ;
#15303 = ORIENTED_EDGE ( 'NONE', *, *, #17219, .T. ) ;
#15304 = SURFACE_STYLE_FILL_AREA ( #2188 ) ;
#15305 = CARTESIAN_POINT ( 'NONE',  ( 18.97648483518030815, 140.5725221174451747, 16.15500418213391143 ) ) ;
#15306 = CARTESIAN_POINT ( 'NONE',  ( -154.9692839938123257, 171.6227766016838245, -23.61711149033413903 ) ) ;
#15307 = EDGE_CURVE ( 'NONE', #15454, #4882, #3556, .T. ) ;
#15308 = DIRECTION ( 'NONE',  ( -0.000000000000000000, -0.000000000000000000, -1.000000000000000000 ) ) ;
#15309 = CARTESIAN_POINT ( 'NONE',  ( 196.0000000000000000, 183.6227766016837961, 5.571800142134975431 ) ) ;
#15310 = PLANE ( 'NONE',  #9528 ) ;
#15311 = VECTOR ( 'NONE', #14979, 1000.000000000000000 ) ;
#15312 = CARTESIAN_POINT ( 'NONE',  ( 22.42614717998981178, 29.85190128815754917, 7.820018500632365033 ) ) ;
#15313 = DIRECTION ( 'NONE',  ( -0.000000000000000000, -0.000000000000000000, 1.000000000000000000 ) ) ;
#15314 = CARTESIAN_POINT ( 'NONE',  ( 48.00000000000000000, 171.6227766016838245, 0.000000000000000000 ) ) ;
#15315 = ORIENTED_EDGE ( 'NONE', *, *, #9995, .T. ) ;
#15316 = ORIENTED_EDGE ( 'NONE', *, *, #3285, .F. ) ;
#15317 = CARTESIAN_POINT ( 'NONE',  ( 32.29171157738787912, 19.99999999999999645, -15.02090973094133375 ) ) ;
#15318 = CARTESIAN_POINT ( 'NONE',  ( -100.0000000000000000, 171.6227766016838245, -27.69059892324149530 ) ) ;
#15319 = ORIENTED_EDGE ( 'NONE', *, *, #1992, .T. ) ;
#15320 = DIRECTION ( 'NONE',  ( 1.000000000000000000, 0.000000000000000000, 0.000000000000000000 ) ) ;
#15321 = LINE ( 'NONE', #16915, #3847 ) ;
#15322 = ORIENTED_EDGE ( 'NONE', *, *, #17160, .T. ) ;
#15323 = CARTESIAN_POINT ( 'NONE',  ( 34.88846745512547187, 152.3168652870157018, -26.76420670456569084 ) ) ;
#15324 = CYLINDRICAL_SURFACE ( 'NONE', #8500, 1.000000000000000888 ) ;
#15325 = EDGE_CURVE ( 'NONE', #16876, #13316, #8949, .T. ) ;
#15326 = EDGE_CURVE ( 'NONE', #3275, #6638, #13203, .T. ) ;
#15327 = EDGE_CURVE ( 'NONE', #11165, #14513, #16933, .T. ) ;
#15328 = FACE_OUTER_BOUND ( 'NONE', #2275, .T. ) ;
#15329 = DIRECTION ( 'NONE',  ( -1.000000000000000000, 0.000000000000000000, 0.000000000000000000 ) ) ;
#15330 = LINE ( 'NONE', #16756, #4580 ) ;
#15331 = CARTESIAN_POINT ( 'NONE',  ( -32.55406425504675383, 119.4745293701281526, 5.163900856522909422 ) ) ;
#15332 = CARTESIAN_POINT ( 'NONE',  ( 40.00000000000000711, 146.6227766016838245, 0.000000000000000000 ) ) ;
#15333 = ORIENTED_EDGE ( 'NONE', *, *, #3215, .F. ) ;
#15334 = DIRECTION ( 'NONE',  ( -1.000000000000000000, -0.000000000000000000, -0.000000000000000000 ) ) ;
#15335 = ORIENTED_EDGE ( 'NONE', *, *, #2237, .F. ) ;
#15336 = CARTESIAN_POINT ( 'NONE',  ( -72.74938895237542624, 194.6575378623844870, -23.63707964515041482 ) ) ;
#15337 = CARTESIAN_POINT ( 'NONE',  ( 27.50000000000000355, 196.6227766016838245, 0.000000000000000000 ) ) ;
#15338 = ORIENTED_EDGE ( 'NONE', *, *, #8571, .F. ) ;
#15339 = DIRECTION ( 'NONE',  ( -1.000000000000000000, 0.000000000000000000, 0.000000000000000000 ) ) ;
#15340 = DIRECTION ( 'NONE',  ( -1.000000000000000000, -0.000000000000000000, 0.000000000000000000 ) ) ;
#15341 = CARTESIAN_POINT ( 'NONE',  ( 16.26529498815395769, 136.8354558863973409, 4.782531348471837696 ) ) ;
#15342 = B_SPLINE_CURVE_WITH_KNOTS ( 'NONE', 3,
 ( #7184, #451, #4545, #8599, #14010, #10004, #7275, #12680, #14103, #553 ),
 .UNSPECIFIED., .F., .F.,
 ( 4, 2, 2, 2, 4 ),
 ( 1.908195823574487804E-17, 0.002588446031580681969, 0.005176892063161340519, 0.007765338094741998202, 0.01035378412632265675 ),
 .UNSPECIFIED. ) ;
#15343 = ORIENTED_EDGE ( 'NONE', *, *, #9138, .F. ) ;
#15344 = DIRECTION ( 'NONE',  ( 8.673617379884036705E-17, -8.673617379884037444E-16, -1.000000000000000000 ) ) ;
#15345 = FACE_OUTER_BOUND ( 'NONE', #4693, .T. ) ;
#15346 = CYLINDRICAL_SURFACE ( 'NONE', #15239, 6.000000000000008882 ) ;
#15347 = LINE ( 'NONE', #11185, #5698 ) ;
#15348 = CARTESIAN_POINT ( 'NONE',  ( 21.36708699129047773, 18.00000000000000000, 23.94811280430834088 ) ) ;
#15349 = PRODUCT_DEFINITION_SHAPE ( 'NONE', 'NONE',  #17526 ) ;
#15350 = DIRECTION ( 'NONE',  ( 0.000000000000000000, 1.000000000000000000, 0.000000000000000000 ) ) ;
#15351 = ORIENTED_EDGE ( 'NONE', *, *, #4352, .T. ) ;
#15352 = CARTESIAN_POINT ( 'NONE',  ( 27.48361012698968864, 138.6227766016838245, -1.063447695028166570E-14 ) ) ;
#15353 = DIRECTION ( 'NONE',  ( 0.000000000000000000, 0.000000000000000000, -1.000000000000000000 ) ) ;
#15354 = VERTEX_POINT ( 'NONE', #7622 ) ;
#15355 = CARTESIAN_POINT ( 'NONE',  ( 49.99999999999998579, 175.6227766016838530, 19.42820660268601074 ) ) ;
#15356 = FACE_BOUND ( 'NONE', #9750, .T. ) ;
#15357 = ORIENTED_EDGE ( 'NONE', *, *, #612, .F. ) ;
#15358 = ORIENTED_EDGE ( 'NONE', *, *, #9046, .T. ) ;
#15359 = DIRECTION ( 'NONE',  ( -0.000000000000000000, -0.000000000000000000, 1.000000000000000000 ) ) ;
#15360 = ORIENTED_EDGE ( 'NONE', *, *, #628, .T. ) ;
#15361 = EDGE_CURVE ( 'NONE', #2062, #5181, #1408, .T. ) ;
#15362 = CYLINDRICAL_SURFACE ( 'NONE', #13217, 20.00000000000000355 ) ;
#15363 = ORIENTED_EDGE ( 'NONE', *, *, #6526, .F. ) ;
#15364 = CARTESIAN_POINT ( 'NONE',  ( -48.00000000000000000, 206.6227766016838245, -2.143131898507868248E-15 ) ) ;
#15365 = CARTESIAN_POINT ( 'NONE',  ( -48.00000000000000000, 191.6227766016837961, -1.224646799147353454E-15 ) ) ;
#15366 = DIRECTION ( 'NONE',  ( 0.000000000000000000, 0.000000000000000000, -1.000000000000000000 ) ) ;
#15367 = CARTESIAN_POINT ( 'NONE',  ( 17.00000000000000000, 206.6227766016838245, -2.143131898507868248E-15 ) ) ;
#15368 = ORIENTED_EDGE ( 'NONE', *, *, #7212, .T. ) ;
#15369 = EDGE_CURVE ( 'NONE', #14777, #6195, #11295, .T. ) ;
#15370 = LINE ( 'NONE', #9798, #11237 ) ;
#15371 = CARTESIAN_POINT ( 'NONE',  ( -100.0000000000000000, 100.0000000000000142, 0.000000000000000000 ) ) ;
#15372 = DIRECTION ( 'NONE',  ( 1.000000000000000000, 0.000000000000000000, 0.000000000000000000 ) ) ;
#15373 = CARTESIAN_POINT ( 'NONE',  ( -12.63609539511577218, 19.99999999999999645, -24.35132453916816431 ) ) ;
#15374 = DIRECTION ( 'NONE',  ( 1.000000000000000000, 0.000000000000000000, 0.000000000000000000 ) ) ;
#15375 = CARTESIAN_POINT ( 'NONE',  ( -34.99999999999999289, 122.0000000000000000, 0.000000000000000000 ) ) ;
#15376 = ORIENTED_EDGE ( 'NONE', *, *, #823, .T. ) ;
#15377 = EDGE_CURVE ( 'NONE', #1349, #3629, #7890, .T. ) ;
#15378 = LINE ( 'NONE', #7496, #7813 ) ;
#15379 = VECTOR ( 'NONE', #11926, 1000.000000000000000 ) ;
#15380 = ORIENTED_EDGE ( 'NONE', *, *, #10556, .F. ) ;
#15381 = SURFACE_STYLE_FILL_AREA ( #11575 ) ;
#15382 = CARTESIAN_POINT ( 'NONE',  ( -85.55670654414588228, 194.3322840258869064, -26.63593000238177666 ) ) ;
#15383 = EDGE_LOOP ( 'NONE', ( #6911, #14196, #11981, #2594 ) ) ;
#15384 = CARTESIAN_POINT ( 'NONE',  ( 39.99999999999998579, 5.659323622547703371E-16, -33.00000000000000000 ) ) ;
#15385 = EDGE_CURVE ( 'NONE', #9656, #13808, #10154, .T. ) ;
#15386 = EDGE_CURVE ( 'NONE', #4348, #2857, #16039, .T. ) ;
#15387 = CARTESIAN_POINT ( 'NONE',  ( -208.1430079281944074, 172.4097984991905435, -5.932774073184737595 ) ) ;
#15388 = EDGE_CURVE ( 'NONE', #12276, #2002, #9026, .T. ) ;
#15389 = ORIENTED_EDGE ( 'NONE', *, *, #17098, .F. ) ;
#15390 = CARTESIAN_POINT ( 'NONE',  ( 34.93420767853316988, 18.00000000000000355, 0.000000000000000000 ) ) ;
#15391 = LINE ( 'NONE', #3620, #12973 ) ;
#15392 = CARTESIAN_POINT ( 'NONE',  ( 24.93507336697364707, 29.86842105263157876, -15.00000000000000000 ) ) ;
#15393 = FACE_BOUND ( 'NONE', #13955, .T. ) ;
#15394 = VECTOR ( 'NONE', #12847, 1000.000000000000114 ) ;
#15395 = ORIENTED_EDGE ( 'NONE', *, *, #16990, .T. ) ;
#15396 = STYLED_ITEM ( 'NONE', ( #2663 ), #11096 ) ;
#15397 = EDGE_LOOP ( 'NONE', ( #16783, #4830, #10835, #11629, #7533, #6546 ) ) ;
#15398 = CARTESIAN_POINT ( 'NONE',  ( 33.88365274872861477, 19.99999999999999645, -11.43011099234506212 ) ) ;
#15399 = CARTESIAN_POINT ( 'NONE',  ( -20.00000000000000355, 171.6227766016838245, -19.49999999999998934 ) ) ;
#15400 = ORIENTED_EDGE ( 'NONE', *, *, #15450, .T. ) ;
#15401 = LINE ( 'NONE', #541, #12066 ) ;
#15402 = LINE ( 'NONE', #894, #8359 ) ;
#15403 = ORIENTED_EDGE ( 'NONE', *, *, #497, .F. ) ;
#15404 = DIRECTION ( 'NONE',  ( 0.000000000000000000, -0.4999999999999997224, 0.8660254037844387076 ) ) ;
#15405 = B_SPLINE_CURVE_WITH_KNOTS ( 'NONE', 3,
 ( #3411, #10031, #14129, #4825, #15691, #11454, #3574, #839, #2155, #2491, #1166, #7887, #7395, #2071, #7555, #12873, #10628, #17032, #12792, #10288, #6567, #15615, #4899, #15533, #15442, #10215 ),
 .UNSPECIFIED., .F., .F.,
 ( 4, 2, 2, 2, 2, 2, 2, 2, 2, 2, 2, 2, 4 ),
 ( 0.000000000000000000, 0.002002783134349993537, 0.004005566268699987074, 0.008011132537399970679, 0.01001391567174996812, 0.01201669880609996383, 0.01602226507479994830, 0.01802504820914994227, 0.02002783134349994318, 0.02403339761219993459, 0.02603618074654993550, 0.02803896388089993641, 0.03204453014959993129 ),
 .UNSPECIFIED. ) ;
#15406 = VECTOR ( 'NONE', #1876, 1000.000000000000000 ) ;
#15407 = CARTESIAN_POINT ( 'NONE',  ( -25.15885279626527549, 18.00000000000000355, 15.13659797665870066 ) ) ;
#15408 = AXIS2_PLACEMENT_3D ( 'NONE', #9642, #9986, #4340 ) ;
#15409 = AXIS2_PLACEMENT_3D ( 'NONE', #2705, #13510, #1380 ) ;
#15410 = DIRECTION ( 'NONE',  ( -1.000000000000000000, -0.000000000000000000, -0.000000000000000000 ) ) ;
#15411 = CYLINDRICAL_SURFACE ( 'NONE', #6353, 3.999999999999999556 ) ;
#15412 = CARTESIAN_POINT ( 'NONE',  ( -7.970809231268917827, 17.99999999998357936, 12.80353734461080428 ) ) ;
#15413 = LINE ( 'NONE', #16578, #4097 ) ;
#15414 = LINE ( 'NONE', #1712, #11438 ) ;
#15415 = VERTEX_POINT ( 'NONE', #8151 ) ;
#15416 = CARTESIAN_POINT ( 'NONE',  ( 49.99999999999998579, 175.6227766016838245, -5.571800142134975431 ) ) ;
#15417 = B_SPLINE_CURVE_WITH_KNOTS ( 'NONE', 3,
 ( #1018, #5098, #15981, #14482, #16974, #2265, #861, #10492, #6168, #2347, #3866, #11563, #17049, #10397, #3687, #7740, #6253, #2436, #14399, #15897 ),
 .UNSPECIFIED., .F., .F.,
 ( 4, 2, 2, 2, 2, 2, 2, 2, 2, 4 ),
 ( 0.000000000000000000, 0.002318945972243265704, 0.003478418958364892268, 0.004637891944486519265, 0.006956837916729771525, 0.009275783888973026386, 0.01159472986121627865, 0.01391367583345953091, 0.01623262180570278490, 0.01855156777794603890 ),
 .UNSPECIFIED. ) ;
#15418 = ORIENTED_EDGE ( 'NONE', *, *, #4925, .T. ) ;
#15419 = CARTESIAN_POINT ( 'NONE',  ( -45.00000000000000000, 130.0000000000000000, 15.00000000000000000 ) ) ;
#15420 = AXIS2_PLACEMENT_3D ( 'NONE', #16530, #10854, #16189 ) ;
#15421 = EDGE_CURVE ( 'NONE', #16427, #570, #15527, .T. ) ;
#15422 = CYLINDRICAL_SURFACE ( 'NONE', #11478, 35.00000000000000000 ) ;
#15423 = EDGE_CURVE ( 'NONE', #1164, #12878, #6201, .T. ) ;
#15424 = AXIS2_PLACEMENT_3D ( 'NONE', #2713, #8100, #1024 ) ;
#15425 = EDGE_CURVE ( 'NONE', #5381, #16355, #5330, .T. ) ;
#15426 = ORIENTED_EDGE ( 'NONE', *, *, #14694, .T. ) ;
#15427 = CARTESIAN_POINT ( 'NONE',  ( 37.50000000000000711, 146.6227766016838245, -13.00000000000000000 ) ) ;
#15428 = VECTOR ( 'NONE', #16078, 1000.000000000000000 ) ;
#15429 = CARTESIAN_POINT ( 'NONE',  ( 24.80291332262510196, 19.99999999999999645, 7.298429162487363620 ) ) ;
#15430 = CARTESIAN_POINT ( 'NONE',  ( 21.38051303314620810, 139.8000659834381736, 14.57605648433057510 ) ) ;
#15431 = ORIENTED_EDGE ( 'NONE', *, *, #7889, .F. ) ;
#15432 = ITEM_DEFINED_TRANSFORMATION ( 'NONE', 'NONE', #6714,  #3583 ) ;
#15433 = DIRECTION ( 'NONE',  ( -0.000000000000000000, -1.000000000000000000, -0.000000000000000000 ) ) ;
#15434 = CARTESIAN_POINT ( 'NONE',  ( 27.44407568426044008, 126.9014170516880284, 4.999999999999997335 ) ) ;
#15435 = CARTESIAN_POINT ( 'NONE',  ( -76.58855154275256893, 192.9634543217044893, 25.17141653689332870 ) ) ;
#15436 = LINE ( 'NONE', #8448, #9922 ) ;
#15437 = DIRECTION ( 'NONE',  ( 0.000000000000000000, 0.000000000000000000, 1.000000000000000000 ) ) ;
#15438 = AXIS2_PLACEMENT_3D ( 'NONE', #4572, #9060, #7723 ) ;
#15439 = CARTESIAN_POINT ( 'NONE',  ( -8.509631953695096840, 18.00000000000455103, -12.55445085332768151 ) ) ;
#15440 = ORIENTED_EDGE ( 'NONE', *, *, #849, .F. ) ;
#15441 = CARTESIAN_POINT ( 'NONE',  ( -74.00000000000001421, 196.6227766016838245, -24.49489742783179125 ) ) ;
#15442 = CARTESIAN_POINT ( 'NONE',  ( -8.719536044788661400, 19.99999999999999645, -24.99999999999999645 ) ) ;
#15443 = EDGE_LOOP ( 'NONE', ( #12336, #15838 ) ) ;
#15444 = CYLINDRICAL_SURFACE ( 'NONE', #12132, 2.499999999999998668 ) ;
#15445 = DIRECTION ( 'NONE',  ( 0.000000000000000000, 0.000000000000000000, -1.000000000000000000 ) ) ;
#15446 = ADVANCED_FACE ( 'NONE', ( #13299 ), #16138, .T. ) ;
#15447 = VERTEX_POINT ( 'NONE', #1346 ) ;
#15448 = EDGE_CURVE ( 'NONE', #3421, #10977, #262, .T. ) ;
#15449 = ORIENTED_EDGE ( 'NONE', *, *, #13843, .F. ) ;
#15450 = EDGE_CURVE ( 'NONE', #2358, #5417, #14965, .T. ) ;
#15451 = VECTOR ( 'NONE', #12156, 1000.000000000000000 ) ;
#15452 = CARTESIAN_POINT ( 'NONE',  ( 1.559999999999998943, 0.000000000000000000, 0.000000000000000000 ) ) ;
#15453 = CIRCLE ( 'NONE', #8383, 2.500000000000002220 ) ;
#15454 = VERTEX_POINT ( 'NONE', #13380 ) ;
#15455 = LINE ( 'NONE', #14219, #506 ) ;
#15456 = VECTOR ( 'NONE', #6088, 1000.000000000000000 ) ;
#15457 = EDGE_LOOP ( 'NONE', ( #10232, #15808, #11886, #3041 ) ) ;
#15458 = CARTESIAN_POINT ( 'NONE',  ( 24.72505082391213804, 141.2912748254776147, -13.00000000000000000 ) ) ;
#15459 = CARTESIAN_POINT ( 'NONE',  ( 12.04170873690402566, 130.2202688438208327, 11.06482237631273868 ) ) ;
#15460 = DIRECTION ( 'NONE',  ( -0.000000000000000000, -0.000000000000000000, 1.000000000000000000 ) ) ;
#15461 = CARTESIAN_POINT ( 'NONE',  ( 30.00000000000001066, 146.6227766016838245, -35.00200000000000244 ) ) ;
#15462 = AXIS2_PLACEMENT_3D ( 'NONE', #14518, #13193, #12294 ) ;
#15463 = ORIENTED_EDGE ( 'NONE', *, *, #16073, .F. ) ;
#15464 = DIRECTION ( 'NONE',  ( -1.000000000000000000, 0.000000000000000000, 0.000000000000000000 ) ) ;
#15465 = DIRECTION ( 'NONE',  ( 0.000000000000000000, 1.000000000000000000, 0.000000000000000000 ) ) ;
#15466 = AXIS2_PLACEMENT_3D ( 'NONE', #9637, #13639, #16556 ) ;
#15467 = CARTESIAN_POINT ( 'NONE',  ( 27.99999999999998224, 9.999999999999998224, -35.00200000000000244 ) ) ;
#15468 = EDGE_CURVE ( 'NONE', #11430, #4227, #7054, .T. ) ;
#15469 = CARTESIAN_POINT ( 'NONE',  ( -14.77653433949313744, 31.60550367499664759, -12.35354907637233701 ) ) ;
#15470 = FILL_AREA_STYLE ('',( #15720 ) ) ;
#15471 = AXIS2_PLACEMENT_3D ( 'NONE', #16265, #6801, #2636 ) ;
#15472 = DIRECTION ( 'NONE',  ( -0.000000000000000000, -0.000000000000000000, -1.000000000000000000 ) ) ;
#15473 = EDGE_LOOP ( 'NONE', ( #1994, #7739 ) ) ;
#15474 = CARTESIAN_POINT ( 'NONE',  ( -168.0000000000000284, 168.3180863238817437, 5.723891464432140808 ) ) ;
#15475 = ORIENTED_EDGE ( 'NONE', *, *, #6808, .F. ) ;
#15476 = AXIS2_PLACEMENT_3D ( 'NONE', #13801, #3984, #9440 ) ;
#15477 = LINE ( 'NONE', #3521, #6798 ) ;
#15478 = AXIS2_PLACEMENT_3D ( 'NONE', #4206, #3948, #1462 ) ;
#15479 = LINE ( 'NONE', #15384, #6465 ) ;
#15480 = DIRECTION ( 'NONE',  ( -1.000000000000000000, -0.000000000000000000, -0.000000000000000000 ) ) ;
#15481 = ORIENTED_EDGE ( 'NONE', *, *, #16579, .F. ) ;
#15482 = CARTESIAN_POINT ( 'NONE',  ( 32.50000000000000000, 196.6227766016838245, -16.00000000000000000 ) ) ;
#15483 = FACE_OUTER_BOUND ( 'NONE', #1303, .T. ) ;
#15484 = CARTESIAN_POINT ( 'NONE',  ( 7.655193733048226257, 144.1839557653416080, -18.33333333333333925 ) ) ;
#15485 = EDGE_CURVE ( 'NONE', #10357, #152, #1683, .T. ) ;
#15486 = CARTESIAN_POINT ( 'NONE',  ( 29.48010637980168269, 202.6059057426778622, -16.28038605903246605 ) ) ;
#15487 = ORIENTED_EDGE ( 'NONE', *, *, #13013, .T. ) ;
#15488 = ORIENTED_EDGE ( 'NONE', *, *, #1766, .T. ) ;
#15489 = CARTESIAN_POINT ( 'NONE',  ( 29.97257796258477569, 19.99999999999999645, -18.20111186907413270 ) ) ;
#15490 = AXIS2_PLACEMENT_3D ( 'NONE', #1062, #8047, #12130 ) ;
#15491 = CARTESIAN_POINT ( 'NONE',  ( 26.92745052348471546, 139.3035600351462904, -6.678622460562388952 ) ) ;
#15492 = ORIENTED_EDGE ( 'NONE', *, *, #2506, .F. ) ;
#15493 = ADVANCED_FACE ( 'NONE', ( #8058, #13645 ), #13469, .F. ) ;
#15494 = FACE_BOUND ( 'NONE', #12555, .T. ) ;
#15495 = EDGE_CURVE ( 'NONE', #10480, #11460, #7767, .T. ) ;
#15496 = CARTESIAN_POINT ( 'NONE',  ( -68.00000000000000000, 171.6227766016838245, -2.602085213965210642E-15 ) ) ;
#15497 = ORIENTED_EDGE ( 'NONE', *, *, #15701, .F. ) ;
#15498 = PRODUCT ( 'Detachable Battery Pack Module', 'Detachable Battery Pack Module', '', ( #5621 ) ) ;
#15499 = DIRECTION ( 'NONE',  ( -1.000000000000000000, 0.000000000000000000, 0.000000000000000000 ) ) ;
#15500 = UNCERTAINTY_MEASURE_WITH_UNIT (LENGTH_MEASURE( 1.000000000000000082E-05 ), #3160, 'distance_accuracy_value', 'NONE');
#15501 = AXIS2_PLACEMENT_3D ( 'NONE', #6586, #15334, #8698 ) ;
#15502 = CIRCLE ( 'NONE', #7030, 5.000000000000007994 ) ;
#15503 = CARTESIAN_POINT ( 'NONE',  ( -207.8765633999775275, 166.2728330025812227, -1.416566613164573774 ) ) ;
#15504 = DIRECTION ( 'NONE',  ( 0.000000000000000000, 0.000000000000000000, -1.000000000000000000 ) ) ;
#15505 = CARTESIAN_POINT ( 'NONE',  ( -11.06002279671335131, 17.99999999999999645, 10.55202560282026703 ) ) ;
#15506 = CARTESIAN_POINT ( 'NONE',  ( -45.00000000000000711, 171.6227766016838245, 19.49999999999998224 ) ) ;
#15507 = CARTESIAN_POINT ( 'NONE',  ( 35.27494917608787972, 201.9542783778900059, -13.00000000000000000 ) ) ;
#15508 = ORIENTED_EDGE ( 'NONE', *, *, #240, .T. ) ;
#15509 = CARTESIAN_POINT ( 'NONE',  ( 25.00000000000000000, 196.6227766016838245, 0.000000000000000000 ) ) ;
#15510 = ORIENTED_EDGE ( 'NONE', *, *, #15803, .T. ) ;
#15511 = CARTESIAN_POINT ( 'NONE',  ( -15.00000000000002487, 120.0000000000000284, 4.999999999999999112 ) ) ;
#15512 = CARTESIAN_POINT ( 'NONE',  ( -24.80114670877659222, 18.00000000000000000, -15.70637264050927051 ) ) ;
#15513 = TOROIDAL_SURFACE ( 'NONE', #1956, 25.00000000000000000, 10.00000000000000000 ) ;
#15514 = ORIENTED_EDGE ( 'NONE', *, *, #34, .T. ) ;
#15515 = DIRECTION ( 'NONE',  ( -0.000000000000000000, -0.000000000000000000, -1.000000000000000000 ) ) ;
#15516 = AXIS2_PLACEMENT_3D ( 'NONE', #3446, #11578, #14239 ) ;
#15517 = ADVANCED_FACE ( 'NONE', ( #16222 ), #14877, .F. ) ;
#15518 = CARTESIAN_POINT ( 'NONE',  ( 19.96520957614361436, 19.99999999999771916, 13.72477420846906249 ) ) ;
#15519 = CARTESIAN_POINT ( 'NONE',  ( 25.87766738269516509, 137.9415577646583415, 9.529521052671011461 ) ) ;
#15520 = EDGE_LOOP ( 'NONE', ( #14860, #5211 ) ) ;
#15521 = CARTESIAN_POINT ( 'NONE',  ( 6.134011831684053284, 142.5209969267753820, 19.44444444444444642 ) ) ;
#15522 = FACE_OUTER_BOUND ( 'NONE', #4312, .T. ) ;
#15523 = VECTOR ( 'NONE', #11497, 1000.000000000000000 ) ;
#15524 = DIRECTION ( 'NONE',  ( 0.000000000000000000, 0.000000000000000000, 1.000000000000000000 ) ) ;
#15525 = ADVANCED_FACE ( 'NONE', ( #9468 ), #16303, .F. ) ;
#15526 = FACE_OUTER_BOUND ( 'NONE', #14793, .T. ) ;
#15527 = CIRCLE ( 'NONE', #558, 2.500000000000000000 ) ;
#15528 = CARTESIAN_POINT ( 'NONE',  ( 25.00000000000000711, 146.6227766016838245, 0.000000000000000000 ) ) ;
#15529 = VECTOR ( 'NONE', #8353, 1000.000000000000000 ) ;
#15530 = ORIENTED_EDGE ( 'NONE', *, *, #13394, .F. ) ;
#15531 = DIRECTION ( 'NONE',  ( 1.000000000000000000, 0.000000000000000000, 0.000000000000000000 ) ) ;
#15532 = EDGE_CURVE ( 'NONE', #12025, #3225, #2707, .T. ) ;
#15533 = CARTESIAN_POINT ( 'NONE',  ( -10.03891356649071653, 19.99999999999999289, -24.87483525495232328 ) ) ;
#15534 = ORIENTED_EDGE ( 'NONE', *, *, #7473, .T. ) ;
#15535 = CARTESIAN_POINT ( 'NONE',  ( -73.00000000000001421, 171.6227766016838245, -19.49999999999999645 ) ) ;
#15536 = FACE_BOUND ( 'NONE', #4174, .T. ) ;
#15537 = ORIENTED_EDGE ( 'NONE', *, *, #1922, .F. ) ;
#15538 = ORIENTED_EDGE ( 'NONE', *, *, #10399, .F. ) ;
#15539 = EDGE_LOOP ( 'NONE', ( #14763, #11146, #6937, #5972 ) ) ;
#15540 = CIRCLE ( 'NONE', #11851, 2.500000000000000000 ) ;
#15541 = ORIENTED_EDGE ( 'NONE', *, *, #13216, .T. ) ;
#15542 = CARTESIAN_POINT ( 'NONE',  ( -206.3689767832464668, 174.5534660175772785, 3.987129972734268168 ) ) ;
#15543 = VECTOR ( 'NONE', #14628, 1000.000000000000000 ) ;
#15544 = VERTEX_POINT ( 'NONE', #8313 ) ;
#15545 = FILL_AREA_STYLE_COLOUR ( '', #14338 ) ;
#15546 = DIRECTION ( 'NONE',  ( -1.000000000000000000, -0.000000000000000000, -0.000000000000000000 ) ) ;
#15547 = CARTESIAN_POINT ( 'NONE',  ( 7.438682885632053932, 133.7774783946093464, 12.91151668396746111 ) ) ;
#15548 = DIRECTION ( 'NONE',  ( 1.000000000000000000, -0.000000000000000000, 0.000000000000000000 ) ) ;
#15549 = EDGE_CURVE ( 'NONE', #5356, #14594, #13829, .T. ) ;
#15550 = EDGE_CURVE ( 'NONE', #15970, #14256, #4436, .T. ) ;
#15551 = CARTESIAN_POINT ( 'NONE',  ( 27.44407568426047561, 138.8271129316868837, 3.666666666666728247 ) ) ;
#15552 = ADVANCED_FACE ( 'NONE', ( #11066 ), #16746, .T. ) ;
#15553 = VERTEX_POINT ( 'NONE', #1775 ) ;
#15554 = LINE ( 'NONE', #3430, #11800 ) ;
#15555 = AXIS2_PLACEMENT_3D ( 'NONE', #5378, #9611, #2969 ) ;
#15556 = VECTOR ( 'NONE', #73, 1000.000000000000000 ) ;
#15557 = LINE ( 'NONE', #12636, #3663 ) ;
#15558 = DIRECTION ( 'NONE',  ( 1.000000000000000000, 0.000000000000000000, -0.000000000000000000 ) ) ;
#15559 = CIRCLE ( 'NONE', #7919, 2.500000000000002220 ) ;
#15560 = CARTESIAN_POINT ( 'NONE',  ( -15.98664213571245440, 31.85373729401663212, -11.16351695777366082 ) ) ;
#15561 = LINE ( 'NONE', #11651, #7508 ) ;
#15562 = LINE ( 'NONE', #7238, #4812 ) ;
#15563 = VERTEX_POINT ( 'NONE', #13728 ) ;
#15564 = DIRECTION ( 'NONE',  ( -1.000000000000000000, 0.000000000000000000, 0.000000000000000000 ) ) ;
#15565 = VECTOR ( 'NONE', #6002, 1000.000000000000000 ) ;
#15566 = EDGE_LOOP ( 'NONE', ( #2909, #10959 ) ) ;
#15567 = DIRECTION ( 'NONE',  ( -1.000000000000000000, 0.000000000000000000, 0.000000000000000000 ) ) ;
#15568 = CIRCLE ( 'NONE', #11039, 33.00000000000000000 ) ;
#15569 = CARTESIAN_POINT ( 'NONE',  ( 39.99999999999999289, 8.000000000000000000, -39.99999999999999289 ) ) ;
#15570 = CARTESIAN_POINT ( 'NONE',  ( 14.79728876016037198, 126.7368160533725643, -7.941237055946955614 ) ) ;
#15571 = ORIENTED_EDGE ( 'NONE', *, *, #1862, .F. ) ;
#15572 = DIRECTION ( 'NONE',  ( -0.000000000000000000, 0.000000000000000000, 1.000000000000000000 ) ) ;
#15573 = DIRECTION ( 'NONE',  ( 0.000000000000000000, 0.000000000000000000, -1.000000000000000000 ) ) ;
#15574 = LINE ( 'NONE', #1047, #16413 ) ;
#15575 = CARTESIAN_POINT ( 'NONE',  ( 24.06750934705105749, 197.5381456772451827, -23.52581655030730445 ) ) ;
#15576 = EDGE_LOOP ( 'NONE', ( #1997, #14659, #12489, #13878 ) ) ;
#15577 = VECTOR ( 'NONE', #12612, 1000.000000000000000 ) ;
#15578 = VERTEX_POINT ( 'NONE', #5756 ) ;
#15579 = CARTESIAN_POINT ( 'NONE',  ( 22.23358001889399205, 29.90326853444953059, -11.84310668804517697 ) ) ;
#15580 = LINE ( 'NONE', #15399, #4992 ) ;
#15581 = VERTEX_POINT ( 'NONE', #9731 ) ;
#15582 = CARTESIAN_POINT ( 'NONE',  ( -50.00000000000000000, 154.3022685259950038, 9.999999999999900524 ) ) ;
#15583 = CARTESIAN_POINT ( 'NONE',  ( 34.93420767853316988, 30.00000000000000000, 0.000000000000000000 ) ) ;
#15584 = ORIENTED_EDGE ( 'NONE', *, *, #4524, .F. ) ;
#15585 = EDGE_CURVE ( 'NONE', #16986, #3929, #10034, .T. ) ;
#15586 = LINE ( 'NONE', #7439, #15819 ) ;
#15587 = ADVANCED_FACE ( 'NONE', ( #11239 ), #7089, .F. ) ;
#15588 = CIRCLE ( 'NONE', #13331, 5.000000000000004441 ) ;
#15589 = CARTESIAN_POINT ( 'NONE',  ( 32.50000000000000711, 146.6227766016838245, -16.00000000000000000 ) ) ;
#15590 = DIRECTION ( 'NONE',  ( 1.000000000000000000, -0.000000000000000000, -0.000000000000000000 ) ) ;
#15591 = CARTESIAN_POINT ( 'NONE',  ( -16.01409026037699945, 32.68451876144969503, 7.109513113881434698 ) ) ;
#15592 = CARTESIAN_POINT ( 'NONE',  ( 27.99999999999998224, 9.999999999999998224, -35.00200000000000244 ) ) ;
#15593 = DIRECTION ( 'NONE',  ( 5.638339401448894059E-16, -0.000000000000000000, -1.000000000000000000 ) ) ;
#15594 = ORIENTED_EDGE ( 'NONE', *, *, #5128, .F. ) ;
#15595 = CYLINDRICAL_SURFACE ( 'NONE', #17496, 2.500000000000000444 ) ;
#15596 = EDGE_LOOP ( 'NONE', ( #2114, #11836, #8837, #1072 ) ) ;
#15597 = DIRECTION ( 'NONE',  ( -0.8571673013836870192, 0.000000000000000000, -0.5150380737757234151 ) ) ;
#15598 = CARTESIAN_POINT ( 'NONE',  ( -27.70723240392776887, 18.00000000000000000, -8.328409877367404235 ) ) ;
#15599 = ORIENTED_EDGE ( 'NONE', *, *, #11689, .F. ) ;
#15600 = DIRECTION ( 'NONE',  ( 0.000000000000000000, -0.8660254037844413721, 0.4999999999999953371 ) ) ;
#15601 = CARTESIAN_POINT ( 'NONE',  ( 21.08563699167523353, 19.99999999999771561, 13.01331479026599602 ) ) ;
#15602 = EDGE_CURVE ( 'NONE', #805, #4320, #4956, .T. ) ;
#15603 = EDGE_LOOP ( 'NONE', ( #6378, #2112 ) ) ;
#15604 = CARTESIAN_POINT ( 'NONE',  ( 35.00000000000000000, 196.6227766016838245, 0.000000000000000000 ) ) ;
#15605 = DIRECTION ( 'NONE',  ( 0.000000000000000000, 0.000000000000000000, -1.000000000000000000 ) ) ;
#15606 = B_SPLINE_CURVE_WITH_KNOTS ( 'NONE', 3,
 ( #6498, #9142, #11890, #14737, #17299, #17480, #9410, #14643, #2516, #6403 ),
 .UNSPECIFIED., .F., .F.,
 ( 4, 2, 2, 2, 4 ),
 ( 1.908195823574487804E-17, 0.002588446031580678066, 0.005176892063161337050, 0.007765338094741995600, 0.01035378412632265502 ),
 .UNSPECIFIED. ) ;
#15607 = ADVANCED_FACE ( 'NONE', ( #12490 ), #2611, .F. ) ;
#15608 = CARTESIAN_POINT ( 'NONE',  ( -98.00000000000000000, 171.6227766016838245, 0.000000000000000000 ) ) ;
#15609 = CARTESIAN_POINT ( 'NONE',  ( 1.559999999999998943, 0.000000000000000000, -1.499999999999997780 ) ) ;
#15610 = DIRECTION ( 'NONE',  ( 1.000000000000000000, 0.000000000000000000, -0.000000000000000000 ) ) ;
#15611 = ADVANCED_FACE ( 'NONE', ( #6357 ), #11752, .T. ) ;
#15612 = ADVANCED_FACE ( 'NONE', ( #1665 ), #11120, .T. ) ;
#15613 = VERTEX_POINT ( 'NONE', #12543 ) ;
#15614 = CARTESIAN_POINT ( 'NONE',  ( -96.00000000000001421, 171.6227766016838245, 0.000000000000000000 ) ) ;
#15615 = CARTESIAN_POINT ( 'NONE',  ( -12.63167751028161589, 20.00000000000000355, -24.35243221814332060 ) ) ;
#15616 = ORIENTED_EDGE ( 'NONE', *, *, #7738, .F. ) ;
#15617 = CARTESIAN_POINT ( 'NONE',  ( 35.31758992237445938, 193.8375574372276162, -27.04711750382526603 ) ) ;
#15618 = FACE_BOUND ( 'NONE', #12983, .T. ) ;
#15619 = ORIENTED_EDGE ( 'NONE', *, *, #9482, .F. ) ;
#15620 = VERTEX_POINT ( 'NONE', #10049 ) ;
#15621 = EDGE_CURVE ( 'NONE', #17286, #216, #1287, .T. ) ;
#15622 = ORIENTED_EDGE ( 'NONE', *, *, #13957, .T. ) ;
#15623 = CARTESIAN_POINT ( 'NONE',  ( -78.82732927925546562, 154.0361450035975395, -27.92332374485730639 ) ) ;
#15624 = ORIENTED_EDGE ( 'NONE', *, *, #13824, .T. ) ;
#15625 = LINE ( 'NONE', #10141, #8210 ) ;
#15626 = FACE_OUTER_BOUND ( 'NONE', #10546, .T. ) ;
#15627 = CARTESIAN_POINT ( 'NONE',  ( -91.33974596215563224, 136.6227766016838245, 0.000000000000000000 ) ) ;
#15628 = CARTESIAN_POINT ( 'NONE',  ( 22.56235622051156042, 18.00000000000113332, 7.873592366086867855 ) ) ;
#15629 = FACE_OUTER_BOUND ( 'NONE', #5923, .T. ) ;
#15630 = ORIENTED_EDGE ( 'NONE', *, *, #2170, .T. ) ;
#15631 = CARTESIAN_POINT ( 'NONE',  ( 49.99999999999998579, 187.6227766016837961, 15.00000337241049486 ) ) ;
#15632 = CARTESIAN_POINT ( 'NONE',  ( -151.6393416600920716, 171.6227766016838245, 25.46898629924947244 ) ) ;
#15633 = DIRECTION ( 'NONE',  ( -1.000000000000000000, 0.000000000000000000, 0.000000000000000000 ) ) ;
#15634 = CARTESIAN_POINT ( 'NONE',  ( -17.11671918504270451, 32.08177433558115865, -9.477319364664337442 ) ) ;
#15635 = DIRECTION ( 'NONE',  ( -0.000000000000000000, -0.000000000000000000, -1.000000000000000000 ) ) ;
#15636 = B_SPLINE_CURVE_WITH_KNOTS ( 'NONE', 3,
 ( #5734, #6078, #13893, #2015, #3076, #9967, #8558, #7232, #16798, #11122, #682, #16540, #3167, #6000, #12729, #1752, #8477, #10146, #11211, #8648, #13969, #5911, #14061, #14227, #11390, #4665, #16721, #412, #4411, #11304, #15294, #4587, #11472, #1925, #16883, #7147, #7323, #4759 ),
 .UNSPECIFIED., .F., .F.,
 ( 4, 2, 2, 2, 2, 2, 2, 2, 2, 2, 2, 2, 2, 2, 2, 2, 2, 2, 4 ),
 ( 0.01870878530979003598, 0.02011211734399855761, 0.02151544937820707576, 0.02432211344662417798, 0.02572544548083270655, 0.02712877751504123164, 0.02783044353214549071, 0.02853210954924975326, 0.02923377556635403315, 0.02993544158345830958, 0.03063710760056260335, 0.03133877361766689018, 0.03204043963477118395, 0.03274210565187547078, 0.03414543768608402363, 0.03554876972029256954, 0.03695210175450111545, 0.03835543378870967524, 0.04116209785712676705 ),
 .UNSPECIFIED. ) ;
#15637 = CARTESIAN_POINT ( 'NONE',  ( 32.06052738088115461, 201.1823876344234066, 14.67159435888867769 ) ) ;
#15638 = EDGE_CURVE ( 'NONE', #7583, #12193, #4585, .T. ) ;
#15639 = EDGE_CURVE ( 'NONE', #11894, #11114, #8474, .T. ) ;
#15640 = ADVANCED_FACE ( 'NONE', ( #4497 ), #5998, .T. ) ;
#15641 = VERTEX_POINT ( 'NONE', #7407 ) ;
#15642 = CARTESIAN_POINT ( 'NONE',  ( -725.0000000000000000, 19.99999999999995737, 0.000000000000000000 ) ) ;
#15643 = VERTEX_POINT ( 'NONE', #13796 ) ;
#15644 = SURFACE_STYLE_USAGE ( .BOTH. , #3441 ) ;
#15645 = LINE ( 'NONE', #7242, #14419 ) ;
#15646 = CARTESIAN_POINT ( 'NONE',  ( -68.00000000000000000, 191.6227766016837961, -1.224646799147353454E-15 ) ) ;
#15647 = CARTESIAN_POINT ( 'NONE',  ( 13.91851620013868995, 127.9827558526829563, -9.294367823883964874 ) ) ;
#15648 = VERTEX_POINT ( 'NONE', #4409 ) ;
#15649 = CARTESIAN_POINT ( 'NONE',  ( 49.99999999999998579, 175.6227766016838530, 21.92820660268601074 ) ) ;
#15650 = CYLINDRICAL_SURFACE ( 'NONE', #14389, 2.499999999999998668 ) ;
#15651 = DIRECTION ( 'NONE',  ( 0.000000000000000000, 0.000000000000000000, 1.000000000000000000 ) ) ;
#15652 = CARTESIAN_POINT ( 'NONE',  ( 32.61283963115067053, 202.0279528788176151, -17.33673759440343076 ) ) ;
#15653 = ORIENTED_EDGE ( 'NONE', *, *, #687, .T. ) ;
#15654 = ORIENTED_EDGE ( 'NONE', *, *, #16261, .T. ) ;
#15655 = CARTESIAN_POINT ( 'NONE',  ( 17.04731744882672828, 19.99999999999885247, -14.80421929169553685 ) ) ;
#15656 = VECTOR ( 'NONE', #660, 1000.000000000000000 ) ;
#15657 = CARTESIAN_POINT ( 'NONE',  ( 40.00000000000000711, 171.6227766016838245, 0.000000000000000000 ) ) ;
#15658 = ADVANCED_FACE ( 'NONE', ( #3073 ), #4662, .F. ) ;
#15659 = ORIENTED_EDGE ( 'NONE', *, *, #78, .T. ) ;
#15660 = DIRECTION ( 'NONE',  ( -1.000000000000000000, 0.000000000000000000, 0.000000000000000000 ) ) ;
#15661 = EDGE_CURVE ( 'NONE', #9691, #2967, #9794, .T. ) ;
#15662 = LINE ( 'NONE', #7607, #9022 ) ;
#15663 = VERTEX_POINT ( 'NONE', #9702 ) ;
#15664 = DIRECTION ( 'NONE',  ( 0.000000000000000000, 0.000000000000000000, 1.000000000000000000 ) ) ;
#15665 = DIRECTION ( 'NONE',  ( -1.000000000000000000, 0.000000000000000000, 0.000000000000000000 ) ) ;
#15666 = CONICAL_SURFACE ( 'NONE', #2675, 2.499999999999998668, 1.029744260000002187 ) ;
#15667 = DIRECTION ( 'NONE',  ( 0.000000000000000000, 0.000000000000000000, 1.000000000000000000 ) ) ;
#15668 = CARTESIAN_POINT ( 'NONE',  ( -12.76199592490470636, 17.99999999999999645, 6.193401609026034649 ) ) ;
#15669 = CIRCLE ( 'NONE', #13419, 25.46898629924947244 ) ;
#15670 = CARTESIAN_POINT ( 'NONE',  ( 25.00000000000000000, 196.6227766016838245, -12.99999999999999822 ) ) ;
#15671 = CARTESIAN_POINT ( 'NONE',  ( 31.77450688729555139, 140.8861252344925106, -16.74142298344134616 ) ) ;
#15672 = ORIENTED_EDGE ( 'NONE', *, *, #1387, .T. ) ;
#15673 = CARTESIAN_POINT ( 'NONE',  ( 40.00000000000000711, 204.6227766016838245, 2.020667218593133100E-15 ) ) ;
#15674 = ORIENTED_EDGE ( 'NONE', *, *, #14584, .F. ) ;
#15675 = EDGE_CURVE ( 'NONE', #5614, #1074, #3341, .T. ) ;
#15676 = DIRECTION ( 'NONE',  ( 0.000000000000000000, 0.000000000000000000, 1.000000000000000000 ) ) ;
#15677 = PLANE ( 'NONE',  #12325 ) ;
#15678 = ORIENTED_EDGE ( 'NONE', *, *, #4273, .F. ) ;
#15679 = DIRECTION ( 'NONE',  ( 0.000000000000000000, 1.000000000000000000, 1.224646799147353207E-16 ) ) ;
#15680 = AXIS2_PLACEMENT_3D ( 'NONE', #16837, #8519, #11256 ) ;
#15681 = CARTESIAN_POINT ( 'NONE',  ( 25.06493225413665016, 20.00000000000000000, 5.000000000000004441 ) ) ;
#15682 = ORIENTED_EDGE ( 'NONE', *, *, #10954, .F. ) ;
#15683 = CARTESIAN_POINT ( 'NONE',  ( 0.000000000000000000, -0.8660254037844428154, -1.499999999999997780 ) ) ;
#15684 = CARTESIAN_POINT ( 'NONE',  ( 0.000000000000000000, 0.000000000000000000, 0.000000000000000000 ) ) ;
#15685 = CARTESIAN_POINT ( 'NONE',  ( -13.49179905494335507, 31.33781166378165395, -13.29076615231557490 ) ) ;
#15686 = CARTESIAN_POINT ( 'NONE',  ( -14.94236098988382722, 32.37030496448370798, -9.276599271047366813 ) ) ;
#15687 = VECTOR ( 'NONE', #309, 1000.000000000000000 ) ;
#15688 = ORIENTED_EDGE ( 'NONE', *, *, #11916, .F. ) ;
#15689 = DIRECTION ( 'NONE',  ( 1.000000000000000000, 0.000000000000000000, -0.000000000000000000 ) ) ;
#15690 = B_SPLINE_CURVE_WITH_KNOTS ( 'NONE', 3,
 ( #13641, #16394, #4259, #2918, #267, #4339, #15484, #7166 ),
 .UNSPECIFIED., .F., .F.,
 ( 4, 2, 2, 4 ),
 ( 0.01981773175714084123, 0.02208185334846130693, 0.02434597493978176916, 0.02887421812242269709 ),
 .UNSPECIFIED. ) ;
#15691 = CARTESIAN_POINT ( 'NONE',  ( -27.70723240392776532, 19.99999999999999289, -8.328409877367407788 ) ) ;
#15692 = EDGE_LOOP ( 'NONE', ( #1316, #15315, #2613, #2776 ) ) ;
#15693 = EDGE_CURVE ( 'NONE', #4419, #4489, #3006, .T. ) ;
#15694 = CARTESIAN_POINT ( 'NONE',  ( 24.86101889991104485, 193.5203449394524853, -27.30457132278911558 ) ) ;
#15695 = CIRCLE ( 'NONE', #8068, 3.999999999999998668 ) ;
#15696 = CARTESIAN_POINT ( 'NONE',  ( -24.99999999999999645, 120.0000000000000284, 0.000000000000000000 ) ) ;
#15697 = AXIS2_PLACEMENT_3D ( 'NONE', #7838, #14570, #13249 ) ;
#15698 = EDGE_LOOP ( 'NONE', ( #2880, #6024, #829, #4461 ) ) ;
#15699 = ORIENTED_EDGE ( 'NONE', *, *, #2749, .T. ) ;
#15700 = VERTEX_POINT ( 'NONE', #331 ) ;
#15701 = EDGE_CURVE ( 'NONE', #14936, #13466, #3831, .T. ) ;
#15702 = EDGE_CURVE ( 'NONE', #11848, #4295, #16535, .T. ) ;
#15703 = CARTESIAN_POINT ( 'NONE',  ( -73.19385591260828505, 149.8074533144823590, -24.76648413410753591 ) ) ;
#15704 = EDGE_CURVE ( 'NONE', #8580, #9736, #7321, .T. ) ;
#15705 = AXIS2_PLACEMENT_3D ( 'NONE', #4817, #13944, #574 ) ;
#15706 = VERTEX_POINT ( 'NONE', #12727 ) ;
#15707 = DIRECTION ( 'NONE',  ( 0.000000000000000000, 0.000000000000000000, 1.000000000000000000 ) ) ;
#15708 = CARTESIAN_POINT ( 'NONE',  ( 13.66341101665266677, 138.6227766016838245, -1.000341871676679184E-14 ) ) ;
#15709 = PRESENTATION_LAYER_ASSIGNMENT (  '', '', ( #157 ) ) ;
#15710 = SURFACE_STYLE_USAGE ( .BOTH. , #10664 ) ;
#15711 = CARTESIAN_POINT ( 'NONE',  ( 24.00000000000000355, 146.6227766016838245, -24.49489742783179480 ) ) ;
#15712 = CARTESIAN_POINT ( 'NONE',  ( -197.9999999999999716, 171.6227766016838245, 8.000000000000007105 ) ) ;
#15713 = CARTESIAN_POINT ( 'NONE',  ( 15.60228996708985072, 124.9392590763940518, 1.450155947765682260E-14 ) ) ;
#15714 = ORIENTED_EDGE ( 'NONE', *, *, #1385, .F. ) ;
#15715 = CARTESIAN_POINT ( 'NONE',  ( 48.00000000000000711, 167.6227766016838530, 8.071800142134975431 ) ) ;
#15716 = DIRECTION ( 'NONE',  ( 1.000000000000000000, 0.000000000000000000, 0.000000000000000000 ) ) ;
#15717 = DIRECTION ( 'NONE',  ( 1.000000000000000000, -0.000000000000000000, -0.000000000000000000 ) ) ;
#15718 = CARTESIAN_POINT ( 'NONE',  ( 24.67988836892261872, 29.87169161469932277, 7.267893787782148785 ) ) ;
#15719 = EDGE_LOOP ( 'NONE', ( #3722, #13131, #15071 ) ) ;
#15720 = FILL_AREA_STYLE_COLOUR ( '', #7779 ) ;
#15721 = VECTOR ( 'NONE', #5430, 1000.000000000000000 ) ;
#15722 = AXIS2_PLACEMENT_3D ( 'NONE', #15965, #5253, #7818 ) ;
#15723 = PRODUCT_RELATED_PRODUCT_CATEGORY ( 'part', '', ( #5593 ) ) ;
#15724 = CARTESIAN_POINT ( 'NONE',  ( 29.74080762574056180, 201.6174249061529338, 13.75941557453018582 ) ) ;
#15725 = ORIENTED_EDGE ( 'NONE', *, *, #7119, .F. ) ;
#15726 = DIRECTION ( 'NONE',  ( 0.000000000000000000, 0.000000000000000000, 1.000000000000000000 ) ) ;
#15727 = CARTESIAN_POINT ( 'NONE',  ( 225.0000000000000000, 89.99999999999997158, -4.999999999999999112 ) ) ;
#15728 = VERTEX_POINT ( 'NONE', #600 ) ;
#15729 =( NAMED_UNIT ( * ) SI_UNIT ( $, .STERADIAN. ) SOLID_ANGLE_UNIT ( ) );
#15730 = LINE ( 'NONE', #2455, #10457 ) ;
#15731 = CIRCLE ( 'NONE', #4709, 20.00000000000000355 ) ;
#15733 = AXIS2_PLACEMENT_3D ( 'NONE', #10095, #3020, #7270 ) ;
#15732 = CARTESIAN_POINT ( 'NONE',  ( -26.89314795393037372, 18.00000000000000000, 11.55702759004479852 ) ) ;
#15734 = DIRECTION ( 'NONE',  ( 0.000000000000000000, 0.000000000000000000, 1.000000000000000000 ) ) ;
#15735 = CIRCLE ( 'NONE', #5281, 750.0000000000000000 ) ;
#15736 = MECHANICAL_DESIGN_GEOMETRIC_PRESENTATION_REPRESENTATION (  '', ( #2461 ), #10934 ) ;
#15737 = LINE ( 'NONE', #10167, #12273 ) ;
#15738 = AXIS2_PLACEMENT_3D ( 'NONE', #6818, #12211, #80 ) ;
#15739 = VERTEX_POINT ( 'NONE', #16796 ) ;
#15740 = CARTESIAN_POINT ( 'NONE',  ( -68.00000000000000000, 171.6227766016838245, 0.000000000000000000 ) ) ;
#15741 = CARTESIAN_POINT ( 'NONE',  ( 48.00000000000000711, 151.6227766016839098, -8.071800142134973655 ) ) ;
#15742 = EDGE_CURVE ( 'NONE', #9093, #489, #1856, .T. ) ;
#15743 = DIRECTION ( 'NONE',  ( -1.000000000000000000, -0.000000000000000000, -0.000000000000000000 ) ) ;
#15744 = CARTESIAN_POINT ( 'NONE',  ( 24.00862450121832126, 196.9927911392394151, -24.11293157882131410 ) ) ;
#15745 = ORIENTED_EDGE ( 'NONE', *, *, #17159, .F. ) ;
#15746 = VERTEX_POINT ( 'NONE', #16881 ) ;
#15747 = CARTESIAN_POINT ( 'NONE',  ( 15.58496356726128873, 29.99118438505512430, -15.00000000000000000 ) ) ;
#15748 = CARTESIAN_POINT ( 'NONE',  ( 39.99999999999998579, -20.00000000000000000, 39.99999999999998579 ) ) ;
#15749 = CONICAL_SURFACE ( 'NONE', #6984, 35.00000000000000000, 0.5235987755983005920 ) ;
#15750 = ORIENTED_EDGE ( 'NONE', *, *, #10951, .F. ) ;
#15751 = MECHANICAL_DESIGN_GEOMETRIC_PRESENTATION_REPRESENTATION (  '', ( #8396 ), #12639 ) ;
#15752 = CARTESIAN_POINT ( 'NONE',  ( -86.00000000000002842, 146.6227766016838245, -35.00000000000000000 ) ) ;
#15753 = VECTOR ( 'NONE', #15994, 1000.000000000000000 ) ;
#15754 = CARTESIAN_POINT ( 'NONE',  ( 13.64704021889961361, 139.0043329719002259, -8.527746218696755420 ) ) ;
#15755 = ORIENTED_EDGE ( 'NONE', *, *, #6132, .F. ) ;
#15756 = CARTESIAN_POINT ( 'NONE',  ( 49.99999999999998579, 191.6227766016837677, 3.071800142134975431 ) ) ;
#15757 = CYLINDRICAL_SURFACE ( 'NONE', #16365, 2.500000000000000444 ) ;
#15758 = CYLINDRICAL_SURFACE ( 'NONE', #10645, 2.500000000000000444 ) ;
#15759 = LINE ( 'NONE', #13194, #3530 ) ;
#15760 = CARTESIAN_POINT ( 'NONE',  ( -8.542481054582452771, 30.38359229753140767, 12.94984885967198451 ) ) ;
#15761 = ADVANCED_FACE ( 'NONE', ( #12982 ), #12316, .T. ) ;
#15762 = EDGE_CURVE ( 'NONE', #9957, #5131, #10144, .T. ) ;
#15763 = B_SPLINE_CURVE_WITH_KNOTS ( 'NONE', 3,
 ( #733, #7540, #3473, #907 ),
 .UNSPECIFIED., .F., .F.,
 ( 4, 4 ),
 ( -6.324563032112924020E-06, 0.0003067249959486639528 ),
 .UNSPECIFIED. ) ;
#15764 = AXIS2_PLACEMENT_3D ( 'NONE', #10695, #2643, #10784 ) ;
#15765 = PLANE ( 'NONE',  #12566 ) ;
#15766 = EDGE_CURVE ( 'NONE', #16968, #7898, #3547, .T. ) ;
#15767 = EDGE_CURVE ( 'NONE', #7515, #15447, #10604, .T. ) ;
#15768 = DIRECTION ( 'NONE',  ( -0.000000000000000000, -0.000000000000000000, 1.000000000000000000 ) ) ;
#15769 = VERTEX_POINT ( 'NONE', #17047 ) ;
#15770 = DIRECTION ( 'NONE',  ( -1.000000000000000000, 0.000000000000000000, 0.000000000000000000 ) ) ;
#15771 = EDGE_LOOP ( 'NONE', ( #14283, #4177 ) ) ;
#15772 = DIRECTION ( 'NONE',  ( 0.000000000000000000, -0.5000000000000011102, -0.8660254037844379305 ) ) ;
#15773 = PLANE ( 'NONE',  #17434 ) ;
#15774 = VERTEX_POINT ( 'NONE', #14302 ) ;
#15775 = CARTESIAN_POINT ( 'NONE',  ( 34.26588824652853305, 20.00000000000000355, 10.16858984204336736 ) ) ;
#15776 = CARTESIAN_POINT ( 'NONE',  ( -20.49999999999998224, 10.00000000000000000, -13.00000000000000000 ) ) ;
#15777 = CARTESIAN_POINT ( 'NONE',  ( 21.54097706593338302, 29.91227807600463606, 12.53500607440986236 ) ) ;
#15778 = VECTOR ( 'NONE', #16289, 999.9999999999998863 ) ;
#15779 = EDGE_LOOP ( 'NONE', ( #13913, #6044, #2420, #3369, #3801 ) ) ;
#15780 = EDGE_CURVE ( 'NONE', #6530, #5523, #6664, .T. ) ;
#15781 = CARTESIAN_POINT ( 'NONE',  ( -151.0000000000000284, 171.6227766016838245, 0.000000000000000000 ) ) ;
#15782 = CARTESIAN_POINT ( 'NONE',  ( 28.54584381417872763, 189.2596037578064738, -27.89172594985640075 ) ) ;
#15783 = DIRECTION ( 'NONE',  ( 0.000000000000000000, 0.000000000000000000, -1.000000000000000000 ) ) ;
#15784 = CARTESIAN_POINT ( 'NONE',  ( -12.80328004468503167, 17.99999999998165734, -5.290760321145399736 ) ) ;
#15785 = ORIENTED_EDGE ( 'NONE', *, *, #11729, .T. ) ;
#15786 = CARTESIAN_POINT ( 'NONE',  ( -7.379000772445021283, 30.00000000000000000, 25.00000000000000000 ) ) ;
#15787 = AXIS2_PLACEMENT_3D ( 'NONE', #5866, #11258, #15062 ) ;
#15788 = ORIENTED_EDGE ( 'NONE', *, *, #15602, .F. ) ;
#15789 = CARTESIAN_POINT ( 'NONE',  ( -73.00000000000001421, 171.6227766016838245, 0.000000000000000000 ) ) ;
#15790 = VECTOR ( 'NONE', #17065, 1000.000000000000000 ) ;
#15791 = CARTESIAN_POINT ( 'NONE',  ( 34.93420767853316988, 18.00000000000000355, 0.000000000000000000 ) ) ;
#15792 = ORIENTED_EDGE ( 'NONE', *, *, #7490, .F. ) ;
#15793 = VERTEX_POINT ( 'NONE', #10393 ) ;
#15794 = ORIENTED_EDGE ( 'NONE', *, *, #10336, .T. ) ;
#15795 = AXIS2_PLACEMENT_3D ( 'NONE', #13349, #15995, #6337 ) ;
#15796 = CARTESIAN_POINT ( 'NONE',  ( -79.40013309498280591, 154.1043103600818256, -27.96613953460096624 ) ) ;
#15797 = AXIS2_PLACEMENT_3D ( 'NONE', #16493, #368, #8692 ) ;
#15798 = ORIENTED_EDGE ( 'NONE', *, *, #1075, .T. ) ;
#15799 = DIRECTION ( 'NONE',  ( 0.000000000000000000, 0.000000000000000000, 1.000000000000000000 ) ) ;
#15800 = EDGE_CURVE ( 'NONE', #12169, #16221, #11906, .T. ) ;
#15801 = AXIS2_PLACEMENT_3D ( 'NONE', #15511, #3126, #5965 ) ;
#15802 = FACE_OUTER_BOUND ( 'NONE', #9496, .T. ) ;
#15803 = EDGE_CURVE ( 'NONE', #4609, #12155, #7481, .T. ) ;
#15804 = PRESENTATION_STYLE_ASSIGNMENT (( #15710 ) ) ;
#15805 = CARTESIAN_POINT ( 'NONE',  ( 27.78002739833986112, 152.2013812635046008, -29.11730325185375534 ) ) ;
#15806 = LINE ( 'NONE', #13067, #185 ) ;
#15807 = CARTESIAN_POINT ( 'NONE',  ( -84.92227909014668796, 147.6670862717896000, 22.70911985051488102 ) ) ;
#15808 = ORIENTED_EDGE ( 'NONE', *, *, #1704, .F. ) ;
#15809 = LINE ( 'NONE', #5182, #6450 ) ;
#15810 = FACE_OUTER_BOUND ( 'NONE', #6401, .T. ) ;
#15811 = DIRECTION ( 'NONE',  ( -0.000000000000000000, -0.000000000000000000, -1.000000000000000000 ) ) ;
#15812 = DIRECTION ( 'NONE',  ( -0.000000000000000000, -1.000000000000000000, -0.000000000000000000 ) ) ;
#15813 = CARTESIAN_POINT ( 'NONE',  ( 22.87571619445694182, 29.89494019521412582, 11.08657135066705379 ) ) ;
#15814 = VERTEX_POINT ( 'NONE', #4914 ) ;
#15815 = DIRECTION ( 'NONE',  ( 1.000000000000000000, 0.000000000000000000, 0.000000000000000000 ) ) ;
#15816 = EDGE_CURVE ( 'NONE', #15563, #2470, #12894, .T. ) ;
#15817 = AXIS2_PLACEMENT_3D ( 'NONE', #10596, #13357, #16006 ) ;
#15818 = VECTOR ( 'NONE', #14359, 1000.000000000000000 ) ;
#15819 = VECTOR ( 'NONE', #3378, 1000.000000000000000 ) ;
#15820 = CARTESIAN_POINT ( 'NONE',  ( 26.35433596972580972, 200.0568792608333410, 16.75365501014454139 ) ) ;
#15821 = EDGE_LOOP ( 'NONE', ( #4290, #8370, #17260, #8622, #323, #15980 ) ) ;
#15822 = LINE ( 'NONE', #14674, #11834 ) ;
#15823 = ORIENTED_EDGE ( 'NONE', *, *, #13939, .T. ) ;
#15824 = DIRECTION ( 'NONE',  ( -0.000000000000000000, -0.000000000000000000, 1.000000000000000000 ) ) ;
#15825 = CARTESIAN_POINT ( 'NONE',  ( 225.0000000000000000, 89.99999999999997158, -4.999999999999999112 ) ) ;
#15826 = AXIS2_PLACEMENT_3D ( 'NONE', #10062, #8748, #3436 ) ;
#15827 = DIRECTION ( 'NONE',  ( 1.000000000000000000, -0.000000000000000000, -0.000000000000000000 ) ) ;
#15828 = VECTOR ( 'NONE', #15040, 1000.000000000000000 ) ;
#15829 = CIRCLE ( 'NONE', #7623, 12.00000000000000000 ) ;
#15830 = CARTESIAN_POINT ( 'NONE',  ( 30.00000000000000355, 196.6227766016838245, 0.000000000000000000 ) ) ;
#15831 = EDGE_LOOP ( 'NONE', ( #5194, #2001, #307, #4019, #5441 ) ) ;
#15832 = DIRECTION ( 'NONE',  ( -1.000000000000000000, 0.000000000000000000, 0.000000000000000000 ) ) ;
#15833 = CARTESIAN_POINT ( 'NONE',  ( -207.4300157105866163, 173.3938951205217904, -4.922080471250932732 ) ) ;
#15834 = DIRECTION ( 'NONE',  ( 1.000000000000000000, 0.000000000000000000, 0.000000000000000000 ) ) ;
#15835 = ADVANCED_FACE ( 'NONE', ( #15629 ), #769, .F. ) ;
#15836 = SURFACE_SIDE_STYLE ('',( #10333 ) ) ;
#15837 = EDGE_CURVE ( 'NONE', #7694, #13835, #8643, .T. ) ;
#15838 = ORIENTED_EDGE ( 'NONE', *, *, #2005, .F. ) ;
#15839 =( BOUNDED_CURVE ( )  B_SPLINE_CURVE ( 3, ( #2357, #7748, #4852, #14408 ),
 .UNSPECIFIED., .F., .F. ) 
 B_SPLINE_CURVE_WITH_KNOTS ( ( 4, 4 ),
 ( 4.792629041327348460, 6.283185307179586232 ),
 .UNSPECIFIED. ) 
 CURVE ( )  GEOMETRIC_REPRESENTATION_ITEM ( )  RATIONAL_B_SPLINE_CURVE ( ( 1.000000000000000000, 0.8232662051119113977, 0.8232662051119113977, 1.000000000000000000 ) ) 
 REPRESENTATION_ITEM ( '' )  );
#15840 = ORIENTED_EDGE ( 'NONE', *, *, #7681, .F. ) ;
#15841 = VERTEX_POINT ( 'NONE', #3506 ) ;
#15842 = VECTOR ( 'NONE', #16406, 1000.000000000000000 ) ;
#15843 = AXIS2_PLACEMENT_3D ( 'NONE', #10235, #14401, #15633 ) ;
#15844 = CARTESIAN_POINT ( 'NONE',  ( 13.88882648224844907, 138.0291231684843751, -11.40862608215692831 ) ) ;
#15845 = EDGE_LOOP ( 'NONE', ( #7359, #8179, #3880, #16588 ) ) ;
#15846 = CARTESIAN_POINT ( 'NONE',  ( -85.89531307607238375, 147.7508872708765750, -25.59654897292657694 ) ) ;
#15847 = AXIS2_PLACEMENT_3D ( 'NONE', #7057, #8111, #12459 ) ;
#15848 = CARTESIAN_POINT ( 'NONE',  ( 10.61972500670372277, 131.6239249143206393, -11.92364046234351527 ) ) ;
#15849 = VERTEX_POINT ( 'NONE', #3765 ) ;
#15850 = ADVANCED_FACE ( 'NONE', ( #9155 ), #6513, .F. ) ;
#15851 = CARTESIAN_POINT ( 'NONE',  ( 49.99999999999998579, 159.6227766016838814, -8.071800142134975431 ) ) ;
#15852 = LINE ( 'NONE', #3903, #852 ) ;
#15853 = CARTESIAN_POINT ( 'NONE',  ( 24.40218896425084338, 201.6348411963793126, -13.74530841833676220 ) ) ;
#15854 = LINE ( 'NONE', #12039, #10072 ) ;
#15855 = CARTESIAN_POINT ( 'NONE',  ( -2.428612866367531510E-15, 18.00000000000000355, 28.00000000000000711 ) ) ;
#15856 = DIRECTION ( 'NONE',  ( -0.000000000000000000, -0.000000000000000000, -1.000000000000000000 ) ) ;
#15857 = CARTESIAN_POINT ( 'NONE',  ( -20.86241502029199424, 18.00000000000000000, 20.14618526197082460 ) ) ;
#15858 = CARTESIAN_POINT ( 'NONE',  ( 35.00000000000000711, 146.6227766016838245, 0.000000000000000000 ) ) ;
#15859 = ORIENTED_EDGE ( 'NONE', *, *, #11264, .T. ) ;
#15860 = CARTESIAN_POINT ( 'NONE',  ( 22.99999999999997868, 9.999999999999998224, 0.000000000000000000 ) ) ;
#15861 = ORIENTED_EDGE ( 'NONE', *, *, #4335, .F. ) ;
#15862 = CARTESIAN_POINT ( 'NONE',  ( -27.98221281347036893, 30.00000000000000355, -4.999999999999999112 ) ) ;
#15863 = LINE ( 'NONE', #16043, #10069 ) ;
#15864 = B_SPLINE_CURVE_WITH_KNOTS ( 'NONE', 3,
 ( #6464, #10713, #14783, #14867, #14517, #8138, #2384, #13549, #6368, #11765, #7780, #11857, #17267, #5141, #1765, #14955, #13637, #5576, #3092, #2914, #9635, #4164, #4334, #11133, #13715, #8572, #9721, #16471, #6824, #16292, #1502, #7162, #8302, #9546, #347, #16553, #3182, #8493, #5486, #15216 ),
 .UNSPECIFIED., .F., .F.,
 ( 4, 2, 2, 2, 2, 2, 2, 2, 2, 2, 2, 2, 2, 2, 2, 2, 2, 2, 2, 4 ),
 ( 0.02243093923957175523, 0.02359459467514160580, 0.02475825011071145984, 0.02592190554628131041, 0.02708556098185116445, 0.02766738869963611402, 0.02824921641742106360, 0.02941287185299096621, 0.03057652728856086882, 0.03115835500634580799, 0.03174018272413074715, 0.03232201044191568284, 0.03290383815970061854, 0.03348566587748556117, 0.03406749359527049686, 0.03523114903084040295, 0.03639480446641030209, 0.03755845990198020123, 0.03872211533755010038, 0.04104942620868985009 ),
 .UNSPECIFIED. ) ;
#15865 = VERTEX_POINT ( 'NONE', #936 ) ;
#15866 = CARTESIAN_POINT ( 'NONE',  ( 50.00000000000000000, 196.6227766016838245, 0.000000000000000000 ) ) ;
#15867 = CARTESIAN_POINT ( 'NONE',  ( 12.31199832339570577, 129.9194306174879046, 10.85217099066659685 ) ) ;
#15868 = VECTOR ( 'NONE', #11447, 1000.000000000000000 ) ;
#15869 = EDGE_CURVE ( 'NONE', #7172, #6658, #15695, .T. ) ;
#15870 = EDGE_CURVE ( 'NONE', #15148, #5896, #12721, .T. ) ;
#15871 = LINE ( 'NONE', #2599, #561 ) ;
#15872 = ADVANCED_FACE ( 'NONE', ( #6945, #14916, #2795 ), #9342, .F. ) ;
#15873 = ORIENTED_EDGE ( 'NONE', *, *, #15034, .F. ) ;
#15874 = DIRECTION ( 'NONE',  ( 1.000000000000000000, -0.000000000000000000, -0.000000000000000000 ) ) ;
#15875 = CARTESIAN_POINT ( 'NONE',  ( 23.65095110843940063, 192.6231533511310943, -25.45681811525070870 ) ) ;
#15876 = CARTESIAN_POINT ( 'NONE',  ( -13.77790586189935951, 31.39781009804136502, -13.10675149387370197 ) ) ;
#15877 = CARTESIAN_POINT ( 'NONE',  ( -11.99122994684827503, 18.00000000000000000, -24.50500383881282573 ) ) ;
#15878 = ORIENTED_EDGE ( 'NONE', *, *, #8063, .F. ) ;
#15879 = CARTESIAN_POINT ( 'NONE',  ( -15.00000000000001421, 130.0000000000000000, -13.00000000000000000 ) ) ;
#15880 = ORIENTED_EDGE ( 'NONE', *, *, #17473, .T. ) ;
#15881 = CARTESIAN_POINT ( 'NONE',  ( 27.79815362222807806, 191.0369151440704343, -29.12214185324409854 ) ) ;
#15882 = DIRECTION ( 'NONE',  ( 2.312964634635742464E-16, 0.000000000000000000, -1.000000000000000000 ) ) ;
#15883 = VERTEX_POINT ( 'NONE', #1286 ) ;
#15884 = ORIENTED_EDGE ( 'NONE', *, *, #11547, .T. ) ;
#15885 = EDGE_LOOP ( 'NONE', ( #16762, #13018, #5172, #5607, #17141, #16744, #14572, #2435, #6123 ) ) ;
#15886 = B_SPLINE_CURVE_WITH_KNOTS ( 'NONE', 3,
 ( #5018, #7671, #6531, #17236, #3973, #9085, #11918, #14672, #11733, #10410 ),
 .UNSPECIFIED., .F., .F.,
 ( 4, 2, 2, 2, 4 ),
 ( 0.000000000000000000, 0.0003951437508621859934, 0.0007902875017243719867, 0.001185431252586558034, 0.001580575003448743973 ),
 .UNSPECIFIED. ) ;
#15887 = CARTESIAN_POINT ( 'NONE',  ( 196.0000000000000000, 159.6227766016838814, -8.071800142134975431 ) ) ;
#15888 = UNCERTAINTY_MEASURE_WITH_UNIT (LENGTH_MEASURE( 1.000000000000000082E-05 ), #8472, 'distance_accuracy_value', 'NONE');
#15889 = ORIENTED_EDGE ( 'NONE', *, *, #4304, .T. ) ;
#15890 = CARTESIAN_POINT ( 'NONE',  ( 30.00000000000000355, 196.6227766016838245, -18.75000000000000000 ) ) ;
#15891 = CARTESIAN_POINT ( 'NONE',  ( -15.96992528024541613, 32.67167891243749978, 7.259156848219323166 ) ) ;
#15892 = CARTESIAN_POINT ( 'NONE',  ( -50.00000000000000000, 171.6227766016838245, -25.00000000000000000 ) ) ;
#15893 = DIRECTION ( 'NONE',  ( -1.000000000000000000, 0.000000000000000000, 0.000000000000000000 ) ) ;
#15894 = CARTESIAN_POINT ( 'NONE',  ( 32.90650748920769075, 18.00000000000000000, 13.87185692903161360 ) ) ;
#15895 = CARTESIAN_POINT ( 'NONE',  ( -208.3486229709906752, 168.0754701982165500, 6.144114920819689907 ) ) ;
#15896 = EDGE_LOOP ( 'NONE', ( #5841, #203, #17432, #988 ) ) ;
#15897 = CARTESIAN_POINT ( 'NONE',  ( 16.17028938446068764, 143.0439382767918346, 16.49999999999050360 ) ) ;
#15898 = CARTESIAN_POINT ( 'NONE',  ( 22.23780067492955936, 29.90321370453013117, -11.83858959072850858 ) ) ;
#15899 = LINE ( 'NONE', #12986, #4263 ) ;
#15900 = CARTESIAN_POINT ( 'NONE',  ( 31.20890926080315353, 18.00000000000000000, 16.64259892333393154 ) ) ;
#15901 = PLANE ( 'NONE',  #10986 ) ;
#15902 = ORIENTED_EDGE ( 'NONE', *, *, #4283, .T. ) ;
#15903 = CARTESIAN_POINT ( 'NONE',  ( 17.00000000000000000, 171.6227766016838245, 0.000000000000000000 ) ) ;
#15904 = EDGE_CURVE ( 'NONE', #13139, #14743, #6789, .T. ) ;
#15905 = LINE ( 'NONE', #14575, #5388 ) ;
#15906 = EDGE_LOOP ( 'NONE', ( #7770, #12534, #8944, #16745 ) ) ;
#15907 = FACE_BOUND ( 'NONE', #12744, .T. ) ;
#15908 = CARTESIAN_POINT ( 'NONE',  ( -168.0000000000000284, 178.2321571572880146, 0.000000000000000000 ) ) ;
#15909 = ORIENTED_EDGE ( 'NONE', *, *, #15377, .F. ) ;
#15910 =( LENGTH_UNIT ( ) NAMED_UNIT ( * ) SI_UNIT ( .MILLI., .METRE. ) );
#15911 = CARTESIAN_POINT ( 'NONE',  ( -80.48051234362822015, 141.6406938050144504, 13.78697217532817554 ) ) ;
#15912 = DIRECTION ( 'NONE',  ( 1.000000000000000000, 6.217248937900877415E-15, 0.000000000000000000 ) ) ;
#15913 = CARTESIAN_POINT ( 'NONE',  ( -75.00938694728593248, 143.2738031352136829, -20.53261660472919559 ) ) ;
#15914 = DIRECTION ( 'NONE',  ( -1.000000000000000000, -0.000000000000000000, 0.000000000000000000 ) ) ;
#15915 = VERTEX_POINT ( 'NONE', #12087 ) ;
#15916 = CARTESIAN_POINT ( 'NONE',  ( -23.00000000000002842, 120.0000000000000284, 4.999999999999999112 ) ) ;
#15917 = CARTESIAN_POINT ( 'NONE',  ( -207.1416055535977705, 173.4984539563251360, -4.752130938829821183 ) ) ;
#15918 = CARTESIAN_POINT ( 'NONE',  ( 48.00000000000000711, 183.6227766016837961, 3.071800142134975431 ) ) ;
#15919 = DIRECTION ( 'NONE',  ( -0.8660254037844378194, -0.5000000000000015543, -0.000000000000000000 ) ) ;
#15920 = VERTEX_POINT ( 'NONE', #6867 ) ;
#15921 = EDGE_CURVE ( 'NONE', #5946, #11995, #16345, .T. ) ;
#15922 = VERTEX_POINT ( 'NONE', #15002 ) ;
#15923 = LINE ( 'NONE', #5305, #16335 ) ;
#15924 = VERTEX_POINT ( 'NONE', #132 ) ;
#15925 = PLANE ( 'NONE',  #16600 ) ;
#15926 = CARTESIAN_POINT ( 'NONE',  ( 9.276452510677492214, 132.6951329324795381, -12.46699917133672741 ) ) ;
#15927 = EDGE_CURVE ( 'NONE', #11033, #16523, #5533, .T. ) ;
#15928 = ORIENTED_EDGE ( 'NONE', *, *, #14888, .T. ) ;
#15929 = CARTESIAN_POINT ( 'NONE',  ( 22.93524650466158832, 29.84210526315789380, 0.000000000000000000 ) ) ;
#15930 = CARTESIAN_POINT ( 'NONE',  ( -38.00000000000000000, 18.00000000000000355, 0.000000000000000000 ) ) ;
#15931 = EDGE_CURVE ( 'NONE', #12504, #11533, #1547, .T. ) ;
#15932 = ADVANCED_FACE ( 'NONE', ( #15979 ), #7927, .F. ) ;
#15933 = CARTESIAN_POINT ( 'NONE',  ( 22.49999999999999645, 197.1893936856111793, -20.88304578468305905 ) ) ;
#15934 = DIRECTION ( 'NONE',  ( 0.000000000000000000, 0.000000000000000000, 1.000000000000000000 ) ) ;
#15935 = CARTESIAN_POINT ( 'NONE',  ( 2.749999999999999112, 0.000000000000000000, 0.000000000000000000 ) ) ;
#15936 =( BOUNDED_SURFACE ( )  B_SPLINE_SURFACE ( 3, 2, ( 
 ( #9673, #4294, #8264 ),
 ( #9497, #8177, #12079 ),
 ( #14908, #9591, #5358 ),
 ( #11010, #17389, #15074 ),
 ( #1537, #10754, #2788 ),
 ( #1373, #16337, #16070 ),
 ( #4037, #13502, #5526 ),
 ( #6777, #12174, #44 ),
 ( #6860, #13592, #124 ),
 ( #12249, #10913, #2951 ),
 ( #6935, #12339, #8345 ),
 ( #13760, #1634, #7032 ),
 ( #7118, #12517, #12780 ),
 ( #12433, #16686, #381 ),
 ( #10017, #3399, #14200 ),
 ( #15430, #13858, #650 ),
 ( #13940, #9854, #1802 ),
 ( #11176, #7197, #12599 ),
 ( #14024, #5874, #15258 ),
 ( #465, #12691, #567 ),
 ( #7286, #4375, #4467 ),
 ( #15519, #11268, #8530 ),
 ( #4555, #9941, #3133 ),
 ( #8794, #8613, #1724 ),
 ( #8707, #16506, #2061 ),
 ( #9764, #15341, #3306 ),
 ( #14116, #5971, #1890 ),
 ( #3216, #306, #5707 ),
 ( #11360, #11092, #15162 ),
 ( #6047, #16770, #3040 ) ),
 .UNSPECIFIED., .F., .F., .F. ) 
 B_SPLINE_SURFACE_WITH_KNOTS ( ( 4, 2, 2, 2, 2, 2, 2, 2, 2, 2, 2, 2, 2, 2, 4 ),
 ( 3, 3 ),
 ( 0.01165250788892074896, 0.01579789672993320987, 0.01787059115043944033, 0.01890693836069255729, 0.01994328557094567078, 0.02408867441195813169, 0.02616136883246436215, 0.02823406325297059261, 0.03030675767347682306, 0.03237945209398305352, 0.03652484093499551443, 0.03859753535550174142, 0.03963388256575485491, 0.04067022977600797534, 0.04481561861702043625 ),
 ( 0.000000000000000000, 1.000000000000000000 ),
 .UNSPECIFIED. ) 
 GEOMETRIC_REPRESENTATION_ITEM ( )  RATIONAL_B_SPLINE_SURFACE ( (
 ( 1.000000000000000000, 0.8819171036881967574, 1.000000000000000000),
 ( 1.000000000000000000, 0.8793942645247267986, 1.000000000000000000),
 ( 1.000000000000000000, 0.8749458316895478704, 1.000000000000000000),
 ( 1.000000000000000000, 0.8656814021268812720, 1.000000000000000000),
 ( 1.000000000000000000, 0.8621600075896179716, 1.000000000000000000),
 ( 1.000000000000000000, 0.8562492930711324002, 1.000000000000000000),
 ( 1.000000000000000000, 0.8541736901085718037, 1.000000000000000000),
 ( 1.000000000000000000, 0.8498659178639272893, 1.000000000000000000),
 ( 1.000000000000000000, 0.8476283308601378907, 1.000000000000000000),
 ( 1.000000000000000000, 0.8360458749412158497, 1.000000000000000000),
 ( 1.000000000000000000, 0.8255221978280062878, 1.000000000000000000),
 ( 1.000000000000000000, 0.8082270345002190437, 1.000000000000000000),
 ( 1.000000000000000000, 0.8022128341710524913, 1.000000000000000000),
 ( 1.000000000000000000, 0.7899684886178014454, 1.000000000000000000),
 ( 1.000000000000000000, 0.7837128169315926707, 1.000000000000000000),
 ( 1.000000000000000000, 0.7710263478624882483, 1.000000000000000000),
 ( 1.000000000000000000, 0.7645952338536526893, 1.000000000000000000),
 ( 1.000000000000000000, 0.7516613202048504361, 1.000000000000000000),
 ( 1.000000000000000000, 0.7451386183437513910, 1.000000000000000000),
 ( 1.000000000000000000, 0.7257808243684673588, 1.000000000000000000),
 ( 1.000000000000000000, 0.7133953845776390690, 1.000000000000000000),
 ( 1.000000000000000000, 0.6965170042221164870, 1.000000000000000000),
 ( 1.000000000000000000, 0.6911767420095684678, 1.000000000000000000),
 ( 1.000000000000000000, 0.6837405640632492343, 1.000000000000000000),
 ( 1.000000000000000000, 0.6813577907325653049, 1.000000000000000000),
 ( 1.000000000000000000, 0.6768117804539316440, 1.000000000000000000),
 ( 1.000000000000000000, 0.6746439590912862716, 1.000000000000000000),
 ( 1.000000000000000000, 0.6645663254999056857, 1.000000000000000000),
 ( 1.000000000000000000, 0.6588263891901358082, 1.000000000000000000),
 ( 1.000000000000000000, 0.6558243695371221982, 1.000000000000000000) ) ) 
 REPRESENTATION_ITEM ( '' )  SURFACE ( )  );
#15937 = CARTESIAN_POINT ( 'NONE',  ( 37.99999999999999289, 20.00000000000000000, 0.000000000000000000 ) ) ;
#15938 = PLANE ( 'NONE',  #4995 ) ;
#15939 = CARTESIAN_POINT ( 'NONE',  ( -80.00000000000002842, 146.6227766016838245, 10.00000000000000178 ) ) ;
#15940 = CARTESIAN_POINT ( 'NONE',  ( -68.00000000000000000, 191.6227766016837961, 1.224646799147353454E-15 ) ) ;
#15941 = DIRECTION ( 'NONE',  ( -0.000000000000000000, 0.000000000000000000, -1.000000000000000000 ) ) ;
#15942 = ORIENTED_EDGE ( 'NONE', *, *, #4180, .F. ) ;
#15943 = CARTESIAN_POINT ( 'NONE',  ( 12.53348921593948972, 131.0729685438566605, -13.11561688552428784 ) ) ;
#15944 = ORIENTED_EDGE ( 'NONE', *, *, #4463, .F. ) ;
#15945 = DIRECTION ( 'NONE',  ( 1.000000000000000000, 0.000000000000000000, 0.000000000000000000 ) ) ;
#15946 = CARTESIAN_POINT ( 'NONE',  ( -21.35874126517689220, 18.00000000000000355, -19.71585776365615317 ) ) ;
#15947 = ORIENTED_EDGE ( 'NONE', *, *, #13803, .F. ) ;
#15948 = LINE ( 'NONE', #3824, #3795 ) ;
#15949 = CARTESIAN_POINT ( 'NONE',  ( 13.35668486245713282, 128.6964509245273405, 9.918424562684259982 ) ) ;
#15950 = ORIENTED_EDGE ( 'NONE', *, *, #7693, .T. ) ;
#15951 = CARTESIAN_POINT ( 'NONE',  ( 17.20299680575017831, 29.96951112202298262, 14.74034971990100296 ) ) ;
#15952 = VECTOR ( 'NONE', #527, 1000.000000000000000 ) ;
#15953 = ORIENTED_EDGE ( 'NONE', *, *, #1918, .T. ) ;
#15954 = AXIS2_PLACEMENT_3D ( 'NONE', #12337, #16504, #9761 ) ;
#15955 = CARTESIAN_POINT ( 'NONE',  ( -32.64269715136552463, 101.2195121951219647, 4.500000000000000000 ) ) ;
#15956 = CARTESIAN_POINT ( 'NONE',  ( 28.82732927925544431, 189.2094081997701096, -27.92332374485732061 ) ) ;
#15957 = LINE ( 'NONE', #8250, #10488 ) ;
#15958 = CARTESIAN_POINT ( 'NONE',  ( -16.24840885328083928, 32.75254598042347709, -6.058899415740283345 ) ) ;
#15959 = ORIENTED_EDGE ( 'NONE', *, *, #497, .T. ) ;
#15960 = PLANE ( 'NONE',  #1645 ) ;
#15961 = EDGE_CURVE ( 'NONE', #489, #9093, #12275, .T. ) ;
#15962 = EDGE_CURVE ( 'NONE', #6874, #15013, #4371, .T. ) ;
#15963 = ORIENTED_EDGE ( 'NONE', *, *, #2784, .T. ) ;
#15964 = CARTESIAN_POINT ( 'NONE',  ( 30.23477484661547621, 190.6230697630494433, -29.39368741583861322 ) ) ;
#15965 = CARTESIAN_POINT ( 'NONE',  ( -80.00000000000001421, 196.6227766016838245, 10.00000000000000178 ) ) ;
#15966 = VECTOR ( 'NONE', #14808, 1000.000000000000114 ) ;
#15967 = ORIENTED_EDGE ( 'NONE', *, *, #3738, .T. ) ;
#15968 = CIRCLE ( 'NONE', #14829, 23.57392898041431195 ) ;
#15969 = ORIENTED_EDGE ( 'NONE', *, *, #13623, .F. ) ;
#15970 = VERTEX_POINT ( 'NONE', #10682 ) ;
#15971 = PLANE ( 'NONE',  #3899 ) ;
#15972 = VERTEX_POINT ( 'NONE', #300 ) ;
#15973 =( LENGTH_UNIT ( ) NAMED_UNIT ( * ) SI_UNIT ( .MILLI., .METRE. ) );
#15974 = FACE_OUTER_BOUND ( 'NONE', #1971, .T. ) ;
#15975 = LINE ( 'NONE', #17215, #6095 ) ;
#15976 = AXIS2_PLACEMENT_3D ( 'NONE', #8023, #14766, #2639 ) ;
#15977 = CARTESIAN_POINT ( 'NONE',  ( -82.50000000000001421, 196.6227766016838245, 10.00000000000000178 ) ) ;
#15978 = CARTESIAN_POINT ( 'NONE',  ( 29.97257796258590901, 18.00000000000000000, 18.20111186907413980 ) ) ;
#15979 = FACE_OUTER_BOUND ( 'NONE', #16938, .T. ) ;
#15980 = ORIENTED_EDGE ( 'NONE', *, *, #10242, .T. ) ;
#15981 = CARTESIAN_POINT ( 'NONE',  ( 27.32038637416026816, 139.0270950805171424, 5.204462201318943215 ) ) ;
#15982 = CARTESIAN_POINT ( 'NONE',  ( 24.41053355130577884, 29.87514852601161763, -8.212591972297857978 ) ) ;
#15983 = EDGE_CURVE ( 'NONE', #12777, #17253, #10856, .T. ) ;
#15984 = EDGE_CURVE ( 'NONE', #10334, #11543, #2949, .T. ) ;
#15985 = CARTESIAN_POINT ( 'NONE',  ( 6.134011831684053284, 134.2062027339443944, 15.00000000000000000 ) ) ;
#15986 = ADVANCED_FACE ( 'NONE', ( #5705 ), #12431, .F. ) ;
#15987 = DIRECTION ( 'NONE',  ( 1.000000000000000000, 0.000000000000000000, 0.000000000000000000 ) ) ;
#15988 = CARTESIAN_POINT ( 'NONE',  ( 20.22393135579957502, 29.92951751662230109, 13.49252536210626197 ) ) ;
#15989 = ORIENTED_EDGE ( 'NONE', *, *, #2779, .T. ) ;
#15990 = FACE_BOUND ( 'NONE', #12943, .T. ) ;
#15991 = CARTESIAN_POINT ( 'NONE',  ( 26.56193816801034302, 200.2660383695261999, 16.39286986631262266 ) ) ;
#15992 = AXIS2_PLACEMENT_3D ( 'NONE', #8561, #16373, #12550 ) ;
#15993 = ORIENTED_EDGE ( 'NONE', *, *, #14418, .F. ) ;
#15994 = DIRECTION ( 'NONE',  ( 1.000000000000000000, 0.000000000000000000, 0.000000000000000000 ) ) ;
#15995 = DIRECTION ( 'NONE',  ( 1.000000000000000000, 0.000000000000000000, -0.000000000000000000 ) ) ;
#15996 = VERTEX_POINT ( 'NONE', #7193 ) ;
#15997 = FACE_OUTER_BOUND ( 'NONE', #16044, .T. ) ;
#15998 = DIRECTION ( 'NONE',  ( 0.000000000000000000, 1.000000000000000000, 0.000000000000000000 ) ) ;
#15999 = LINE ( 'NONE', #151, #11545 ) ;
#16000 = ADVANCED_FACE ( 'NONE', ( #2633 ), #2948, .F. ) ;
#16001 = DIRECTION ( 'NONE',  ( -1.000000000000000000, 0.000000000000000000, 0.000000000000000000 ) ) ;
#16002 = AXIS2_PLACEMENT_3D ( 'NONE', #2945, #15154, #16332 ) ;
#16003 = AXIS2_PLACEMENT_3D ( 'NONE', #11882, #2146, #2505 ) ;
#16004 = ORIENTED_EDGE ( 'NONE', *, *, #10059, .F. ) ;
#16005 = CARTESIAN_POINT ( 'NONE',  ( 15.78015847649388448, 143.0439382767918346, 16.49999999999050360 ) ) ;
#16006 = DIRECTION ( 'NONE',  ( 0.000000000000000000, 0.000000000000000000, 1.000000000000000000 ) ) ;
#16007 = CIRCLE ( 'NONE', #15150, 25.69059892324149175 ) ;
#16008 = DIRECTION ( 'NONE',  ( -1.000000000000000000, -0.000000000000000000, -0.000000000000000000 ) ) ;
#16009 = UNCERTAINTY_MEASURE_WITH_UNIT (LENGTH_MEASURE( 1.000000000000000082E-05 ), #6009, 'distance_accuracy_value', 'NONE');
#16010 = CARTESIAN_POINT ( 'NONE',  ( 36.00000000000000711, 196.6227766016838245, -24.49489742783179125 ) ) ;
#16011 = VECTOR ( 'NONE', #12289, 1000.000000000000000 ) ;
#16012 = ORIENTED_EDGE ( 'NONE', *, *, #8189, .T. ) ;
#16013 = ORIENTED_EDGE ( 'NONE', *, *, #3322, .T. ) ;
#16014 = CARTESIAN_POINT ( 'NONE',  ( 0.000000000000000000, 2.000000000000000000, 0.000000000000000000 ) ) ;
#16015 = B_SPLINE_CURVE_WITH_KNOTS ( 'NONE', 3,
 ( #922, #7911, #17034, #7817, #3751, #6310, #15617, #8969, #4827, #9141, #2418, #6237, #10378, #14288, #2248, #11797, #4901, #13224, #15964, #5168, #14545, #7722, #10217, #13056, #11630, #15881, #16959, #13132, #9233, #3492, #10290, #3671, #14465, #1000, #15694, #1095, #7641, #6497, #11889, #11703, #3844, #6149, #14380, #17203 ),
 .UNSPECIFIED., .F., .F.,
 ( 4, 2, 2, 2, 2, 2, 2, 2, 2, 2, 2, 2, 2, 2, 2, 2, 2, 2, 2, 2, 2, 4 ),
 ( 0.000000000000000000, 0.002715240924237344918, 0.003394051155296696869, 0.004072861386356049253, 0.005430481848474700245, 0.006788102310593352971, 0.008145722772712003096, 0.009503343234830655822, 0.01018215346588999259, 0.01086096369694932937, 0.01153977392800866614, 0.01221858415906799944, 0.01289739439012733795, 0.01357620462118667472, 0.01493382508330533785, 0.01629144554542400272, 0.01697025577648333602, 0.01764906600754266586, 0.01900668646966133246, 0.01968549670072063801, 0.02036430693177994009, 0.02172192739389855118 ),
 .UNSPECIFIED. ) ;
#16016 = VERTEX_POINT ( 'NONE', #210 ) ;
#16017 = CARTESIAN_POINT ( 'NONE',  ( -81.58454895572883458, 152.4141840272156116, -29.25805444611330586 ) ) ;
#16018 = CARTESIAN_POINT ( 'NONE',  ( 13.23724818701971984, 139.1606502921264905, -9.139539437136660283 ) ) ;
#16019 = TOROIDAL_SURFACE ( 'NONE', #11209, -78.75916623668499028, 108.0000000000000142 ) ;
#16020 = VERTEX_POINT ( 'NONE', #5871 ) ;
#16021 = CARTESIAN_POINT ( 'NONE',  ( -43.00000000000000000, 144.1839557653416080, -18.33333333333335702 ) ) ;
#16022 = CIRCLE ( 'NONE', #8103, 7.500000000000020428 ) ;
#16023 = DIRECTION ( 'NONE',  ( 0.000000000000000000, 8.410780489584519664E-16, -1.000000000000000000 ) ) ;
#16024 = CARTESIAN_POINT ( 'NONE',  ( -3.000000000000000888, 171.6227766016838245, 0.000000000000000000 ) ) ;
#16025 = DIRECTION ( 'NONE',  ( -0.000000000000000000, -0.000000000000000000, -1.000000000000000000 ) ) ;
#16026 = ADVANCED_FACE ( 'NONE', ( #8438 ), #8342, .T. ) ;
#16027 = CARTESIAN_POINT ( 'NONE',  ( 30.00000000000001066, 146.6227766016838245, -13.00000000000000000 ) ) ;
#16028 = CARTESIAN_POINT ( 'NONE',  ( 21.54590827305403877, 18.00000000000000000, -9.735228713654757726 ) ) ;
#16029 = DIRECTION ( 'NONE',  ( -1.541976423090495387E-16, 0.000000000000000000, -1.000000000000000000 ) ) ;
#16030 = DIRECTION ( 'NONE',  ( 1.000000000000000000, 1.156482317317868274E-16, 0.000000000000000000 ) ) ;
#16031 = DIRECTION ( 'NONE',  ( -0.000000000000000000, -0.000000000000000000, 1.000000000000000000 ) ) ;
#16032 = DIRECTION ( 'NONE',  ( -1.000000000000000000, -0.000000000000000000, -0.000000000000000000 ) ) ;
#16033 = ORIENTED_EDGE ( 'NONE', *, *, #9107, .F. ) ;
#16034 = CARTESIAN_POINT ( 'NONE',  ( 7.674484246658608733, 133.8653086123773903, -14.91481465347803415 ) ) ;
#16035 = LINE ( 'NONE', #6147, #16147 ) ;
#16036 = VECTOR ( 'NONE', #13719, 1000.000000000000000 ) ;
#16037 = ORIENTED_EDGE ( 'NONE', *, *, #9137, .F. ) ;
#16038 = EDGE_CURVE ( 'NONE', #11342, #8547, #379, .T. ) ;
#16039 = LINE ( 'NONE', #10724, #3665 ) ;
#16040 = EDGE_CURVE ( 'NONE', #12106, #7374, #4291, .T. ) ;
#16041 = AXIS2_PLACEMENT_3D ( 'NONE', #12105, #2890, #8109 ) ;
#16042 = EDGE_CURVE ( 'NONE', #14845, #15774, #8016, .T. ) ;
#16043 = CARTESIAN_POINT ( 'NONE',  ( -75.00000000000002842, 146.6227766016838245, -35.00200000000000244 ) ) ;
#16044 = EDGE_LOOP ( 'NONE', ( #2942, #10521, #4834, #11686 ) ) ;
#16045 = CARTESIAN_POINT ( 'NONE',  ( -8.091731396663927711, 30.16237610810089365, 15.00000000000000355 ) ) ;
#16046 = CARTESIAN_POINT ( 'NONE',  ( 27.42233521511133887, 138.9393305618597481, 4.670371664028303726 ) ) ;
#16047 = EDGE_CURVE ( 'NONE', #10334, #15865, #13425, .T. ) ;
#16048 = ORIENTED_EDGE ( 'NONE', *, *, #12848, .F. ) ;
#16049 = CARTESIAN_POINT ( 'NONE',  ( 39.99999999999998579, 4.000000000000000000, -33.00000000000000000 ) ) ;
#16050 = ORIENTED_EDGE ( 'NONE', *, *, #623, .F. ) ;
#16051 = AXIS2_PLACEMENT_3D ( 'NONE', #15740, #13175, #17248 ) ;
#16052 = PRODUCT_DEFINITION_FORMATION_WITH_SPECIFIED_SOURCE ( 'ANY', '', #7438, .NOT_KNOWN. ) ;
#16053 = DIRECTION ( 'NONE',  ( 1.000000000000000000, 0.000000000000000000, -0.000000000000000000 ) ) ;
#16054 = CIRCLE ( 'NONE', #15198, 2.499999999999998668 ) ;
#16055 = CARTESIAN_POINT ( 'NONE',  ( 32.26120111208032171, 189.4484344766680692, -27.77174765869275319 ) ) ;
#16056 = DIRECTION ( 'NONE',  ( 0.000000000000000000, 1.000000000000000000, 0.000000000000000000 ) ) ;
#16057 = CARTESIAN_POINT ( 'NONE',  ( -9.925381735234191538, 18.00000000000231992, -11.63955885304398130 ) ) ;
#16058 = VERTEX_POINT ( 'NONE', #11005 ) ;
#16059 = CARTESIAN_POINT ( 'NONE',  ( 34.23838175495608027, 149.2800176679284903, 24.28646496670947741 ) ) ;
#16060 = VERTEX_POINT ( 'NONE', #7113 ) ;
#16061 = CARTESIAN_POINT ( 'NONE',  ( -84.26947555605805462, 190.4340272497385342, -27.11642929875283414 ) ) ;
#16062 = CARTESIAN_POINT ( 'NONE',  ( -7.379000772444994638, 20.00000000000000000, -25.00000000000000000 ) ) ;
#16063 = EDGE_CURVE ( 'NONE', #11263, #2271, #7029, .T. ) ;
#16064 = EDGE_LOOP ( 'NONE', ( #17111, #13665 ) ) ;
#16065 = CIRCLE ( 'NONE', #799, 2.500000000000002220 ) ;
#16066 = ORIENTED_EDGE ( 'NONE', *, *, #9868, .F. ) ;
#16067 = ORIENTED_EDGE ( 'NONE', *, *, #14606, .F. ) ;
#16068 = VECTOR ( 'NONE', #1893, 1000.000000000000000 ) ;
#16069 =( GEOMETRIC_REPRESENTATION_CONTEXT ( 3 ) GLOBAL_UNCERTAINTY_ASSIGNED_CONTEXT ( ( #5203 ) ) GLOBAL_UNIT_ASSIGNED_CONTEXT ( ( #2996, #16382, #9717 ) ) REPRESENTATION_CONTEXT ( 'NONE', 'WORKASPACE' ) );
#16070 = CARTESIAN_POINT ( 'NONE',  ( 9.474973892937489595, 133.0798911729450538, 14.49933486760529355 ) ) ;
#16071 = ORIENTED_EDGE ( 'NONE', *, *, #3325, .F. ) ;
#16072 = DIRECTION ( 'NONE',  ( 1.000000000000000000, 0.000000000000000000, 0.000000000000000000 ) ) ;
#16073 = EDGE_CURVE ( 'NONE', #11660, #16675, #13982, .T. ) ;
#16074 = CARTESIAN_POINT ( 'NONE',  ( 13.63270490666629975, 138.8028880870465969, -3.449993069226409581 ) ) ;
#16075 = CARTESIAN_POINT ( 'NONE',  ( -11.03695849842137910, 30.81357570984703642, 14.42948753805835871 ) ) ;
#16076 = CARTESIAN_POINT ( 'NONE',  ( 32.98178886359406903, 151.8338245663404393, -28.86895077895843897 ) ) ;
#16077 = LINE ( 'NONE', #5266, #12754 ) ;
#16078 = DIRECTION ( 'NONE',  ( -0.000000000000000000, -0.000000000000000000, -1.000000000000000000 ) ) ;
#16079 = VECTOR ( 'NONE', #7977, 1000.000000000000000 ) ;
#16080 = CIRCLE ( 'NONE', #12689, 2.500000000000000444 ) ;
#16081 = ADVANCED_BREP_SHAPE_REPRESENTATION ( '', ( #11181, #3583 ), #12078 ) ;
#16082 = ORIENTED_EDGE ( 'NONE', *, *, #5474, .F. ) ;
#16083 = PLANE ( 'NONE',  #8143 ) ;
#16084 = CARTESIAN_POINT ( 'NONE',  ( 24.67988836892261872, 29.87169161469932277, -7.267893787782148785 ) ) ;
#16085 = CARTESIAN_POINT ( 'NONE',  ( 15.00000000000000000, 143.0344144757318929, -16.50549856913627877 ) ) ;
#16086 = CARTESIAN_POINT ( 'NONE',  ( -155.0000000000000284, 171.6227766016838245, -21.61734737250326077 ) ) ;
#16087 = CARTESIAN_POINT ( 'NONE',  ( 40.00000000000000711, 171.6227766016838245, 0.000000000000000000 ) ) ;
#16088 = VERTEX_POINT ( 'NONE', #5284 ) ;
#16089 = LINE ( 'NONE', #1121, #998 ) ;
#16090 = DIRECTION ( 'NONE',  ( -0.000000000000000000, -0.000000000000000000, -1.000000000000000000 ) ) ;
#16091 = CIRCLE ( 'NONE', #5916, 2.500000000000000444 ) ;
#16092 = CARTESIAN_POINT ( 'NONE',  ( 32.99999999999998579, 9.999999999999998224, 28.00000000000001066 ) ) ;
#16093 = CIRCLE ( 'NONE', #9876, 27.69059892324149530 ) ;
#16094 = ORIENTED_EDGE ( 'NONE', *, *, #6528, .T. ) ;
#16095 = SURFACE_SIDE_STYLE ('',( #10685 ) ) ;
#16096 = AXIS2_PLACEMENT_3D ( 'NONE', #10839, #13866, #7038 ) ;
#16097 = EDGE_LOOP ( 'NONE', ( #13558, #14885, #5999, #9844 ) ) ;
#16098 = EDGE_CURVE ( 'NONE', #5825, #14287, #14536, .T. ) ;
#16099 = EDGE_CURVE ( 'NONE', #8531, #17520, #15159, .T. ) ;
#16100 = LINE ( 'NONE', #5290, #5087 ) ;
#16101 = EDGE_CURVE ( 'NONE', #7175, #17476, #15256, .T. ) ;
#16102 = CARTESIAN_POINT ( 'NONE',  ( 20.42763382733058108, 18.00000000000000000, -24.23318166603144164 ) ) ;
#16103 = EDGE_CURVE ( 'NONE', #925, #14757, #16590, .T. ) ;
#16104 = DIRECTION ( 'NONE',  ( -0.000000000000000000, 0.000000000000000000, -1.000000000000000000 ) ) ;
#16105 = EDGE_CURVE ( 'NONE', #1310, #11867, #8597, .T. ) ;
#16106 = CARTESIAN_POINT ( 'NONE',  ( -25.15885279626527193, 20.00000000000000355, 15.13659797665870776 ) ) ;
#16107 = ORIENTED_EDGE ( 'NONE', *, *, #4081, .F. ) ;
#16108 = DIRECTION ( 'NONE',  ( 1.000000000000000000, -0.000000000000000000, -0.000000000000000000 ) ) ;
#16109 = VECTOR ( 'NONE', #8213, 1000.000000000000000 ) ;
#16110 = DIRECTION ( 'NONE',  ( 0.000000000000000000, 0.000000000000000000, 1.000000000000000000 ) ) ;
#16111 = AXIS2_PLACEMENT_3D ( 'NONE', #14194, #9122, #14525 ) ;
#16112 = DIRECTION ( 'NONE',  ( -0.000000000000000000, -0.000000000000000000, -1.000000000000000000 ) ) ;
#16113 = VECTOR ( 'NONE', #2186, 1000.000000000000000 ) ;
#16114 = CARTESIAN_POINT ( 'NONE',  ( -103.0000000000000142, 171.6227766016838245, 0.000000000000000000 ) ) ;
#16115 = PRODUCT_DEFINITION_CONTEXT ( 'detailed design', #3142, 'design' ) ;
#16116 = ORIENTED_EDGE ( 'NONE', *, *, #16261, .F. ) ;
#16117 = CARTESIAN_POINT ( 'NONE',  ( 10.45945364060320237, 139.0001874602887995, -13.88305366436908272 ) ) ;
#16118 = ORIENTED_EDGE ( 'NONE', *, *, #3707, .T. ) ;
#16119 = CARTESIAN_POINT ( 'NONE',  ( -85.72918267991042285, 148.4136790374692509, -26.19897850971620912 ) ) ;
#16120 = CARTESIAN_POINT ( 'NONE',  ( 10.22516481506617581, 140.0471213951830407, -11.75777818883246617 ) ) ;
#16121 = AXIS2_PLACEMENT_3D ( 'NONE', #3365, #13178, #6187 ) ;
#16122 = EDGE_LOOP ( 'NONE', ( #3329, #12088, #7746, #10796 ) ) ;
#16123 = CARTESIAN_POINT ( 'NONE',  ( -15.00000000000001421, 20.00000000000004263, -4.999999999999999112 ) ) ;
#16124 = LINE ( 'NONE', #10707, #12161 ) ;
#16125 = VECTOR ( 'NONE', #3357, 1000.000000000000000 ) ;
#16126 = CARTESIAN_POINT ( 'NONE',  ( -168.0000000000000284, 168.3180863238817437, 5.723891464432140808 ) ) ;
#16127 = CARTESIAN_POINT ( 'NONE',  ( -50.00000000000000000, 171.6227766016838245, -25.00000000000000000 ) ) ;
#16128 = CARTESIAN_POINT ( 'NONE',  ( 20.13757169487763576, 18.00000000000000000, -24.32197800972832624 ) ) ;
#16129 = CARTESIAN_POINT ( 'NONE',  ( 32.29171157743327569, 18.00000000000000000, -15.02090973096405158 ) ) ;
#16130 = CARTESIAN_POINT ( 'NONE',  ( -3.000000000000002665, 134.2062027339443944, -25.00000000000000000 ) ) ;
#16131 = CARTESIAN_POINT ( 'NONE',  ( -725.0000000000000000, 19.99999999999995737, 15.00000000000000000 ) ) ;
#16132 = CARTESIAN_POINT ( 'NONE',  ( 49.99999999999998579, 187.6227766016837961, -12.50000337241049309 ) ) ;
#16133 = DIRECTION ( 'NONE',  ( 0.000000000000000000, 0.000000000000000000, -1.000000000000000000 ) ) ;
#16134 = ORIENTED_EDGE ( 'NONE', *, *, #3359, .T. ) ;
#16135 = LINE ( 'NONE', #8149, #16079 ) ;
#16136 = VECTOR ( 'NONE', #10053, 1000.000000000000000 ) ;
#16137 = EDGE_LOOP ( 'NONE', ( #14452, #14738, #2489, #17247 ) ) ;
#16138 = PLANE ( 'NONE',  #10438 ) ;
#16139 = CIRCLE ( 'NONE', #2842, 2.500000000000002220 ) ;
#16140 = DIRECTION ( 'NONE',  ( -0.000000000000000000, -1.000000000000000000, -0.000000000000000000 ) ) ;
#16141 = ORIENTED_EDGE ( 'NONE', *, *, #15962, .F. ) ;
#16142 = ADVANCED_FACE ( 'NONE', ( #16939 ), #3397, .F. ) ;
#16143 = CARTESIAN_POINT ( 'NONE',  ( -11.18069906337402664, 30.84474844633047397, 14.38199110044527274 ) ) ;
#16144 = CARTESIAN_POINT ( 'NONE',  ( 19.90854668962690255, 142.0789032940274410, 14.70609183182490298 ) ) ;
#16145 = ORIENTED_EDGE ( 'NONE', *, *, #7134, .F. ) ;
#16146 = CARTESIAN_POINT ( 'NONE',  ( -95.00000000000000000, 171.6227766016838245, -27.69059892324149530 ) ) ;
#16147 = VECTOR ( 'NONE', #11542, 1000.000000000000000 ) ;
#16148 = ORIENTED_EDGE ( 'NONE', *, *, #16099, .F. ) ;
#16149 = VECTOR ( 'NONE', #4726, 1000.000000000000000 ) ;
#16150 = DIRECTION ( 'NONE',  ( 1.000000000000000000, 0.000000000000000000, -0.000000000000000000 ) ) ;
#16151 = CARTESIAN_POINT ( 'NONE',  ( -207.9328752093750836, 175.6269124087689590, 3.902437508284943846 ) ) ;
#16152 = CARTESIAN_POINT ( 'NONE',  ( 34.99999999999999289, 8.000000000000000000, -39.99999999999999289 ) ) ;
#16153 = DIRECTION ( 'NONE',  ( 0.000000000000000000, 0.000000000000000000, 1.000000000000000000 ) ) ;
#16154 = EDGE_LOOP ( 'NONE', ( #6111, #528, #13088, #9645 ) ) ;
#16155 = CARTESIAN_POINT ( 'NONE',  ( 25.46873702927104333, 148.7415597018667199, 23.77993541092453711 ) ) ;
#16156 = ORIENTED_EDGE ( 'NONE', *, *, #14013, .T. ) ;
#16157 = CARTESIAN_POINT ( 'NONE',  ( -82.81385839426211248, 189.6648409365396333, -27.63145166803556663 ) ) ;
#16158 = CARTESIAN_POINT ( 'NONE',  ( -5.000000000000004441, 142.8100939375178200, 16.63501009223129756 ) ) ;
#16159 = VECTOR ( 'NONE', #477, 1000.000000000000000 ) ;
#16160 = ORIENTED_EDGE ( 'NONE', *, *, #14638, .F. ) ;
#16161 = ORIENTED_EDGE ( 'NONE', *, *, #12092, .T. ) ;
#16162 = ORIENTED_EDGE ( 'NONE', *, *, #3422, .F. ) ;
#16163 = EDGE_CURVE ( 'NONE', #5246, #6881, #3233, .T. ) ;
#16164 = DIRECTION ( 'NONE',  ( -0.000000000000000000, -0.000000000000000000, -1.000000000000000000 ) ) ;
#16165 = EDGE_CURVE ( 'NONE', #5035, #2441, #16811, .T. ) ;
#16166 = VERTEX_POINT ( 'NONE', #7627 ) ;
#16167 = DIRECTION ( 'NONE',  ( -1.000000000000000000, -0.000000000000000000, -0.000000000000000000 ) ) ;
#16168 = EDGE_CURVE ( 'NONE', #4330, #8060, #4088, .T. ) ;
#16169 = CYLINDRICAL_SURFACE ( 'NONE', #166, 2.499999999999998668 ) ;
#16170 = EDGE_CURVE ( 'NONE', #17487, #8812, #6329, .T. ) ;
#16171 = CARTESIAN_POINT ( 'NONE',  ( 22.93524650466160963, 29.84210526315773748, -4.999999999999999112 ) ) ;
#16172 = VECTOR ( 'NONE', #9839, 1000.000000000000000 ) ;
#16173 = DIRECTION ( 'NONE',  ( 0.000000000000000000, 0.000000000000000000, -1.000000000000000000 ) ) ;
#16174 = CARTESIAN_POINT ( 'NONE',  ( -78.65474156909843373, 151.4423111973152061, 26.11038153352143709 ) ) ;
#16175 = ORIENTED_EDGE ( 'NONE', *, *, #15485, .F. ) ;
#16176 = DIRECTION ( 'NONE',  ( 0.000000000000000000, -1.000000000000000000, 0.000000000000000000 ) ) ;
#16177 = CARTESIAN_POINT ( 'NONE',  ( 21.54624641763228254, 29.91220938647573391, -12.53033468027509478 ) ) ;
#16178 = DIRECTION ( 'NONE',  ( 1.000000000000000000, -0.000000000000000000, -0.000000000000000000 ) ) ;
#16179 = DIRECTION ( 'NONE',  ( 0.000000000000000000, 0.000000000000000000, 1.000000000000000000 ) ) ;
#16180 = CARTESIAN_POINT ( 'NONE',  ( -95.00000000000000000, 199.3133755249253056, 1.695560166891042033E-15 ) ) ;
#16181 = CARTESIAN_POINT ( 'NONE',  ( -86.65543510501046853, 143.1309386941324817, -16.67123533649923317 ) ) ;
#16182 = EDGE_CURVE ( 'NONE', #14819, #11143, #7451, .T. ) ;
#16183 = DIRECTION ( 'NONE',  ( -1.000000000000000000, -0.000000000000000000, 0.000000000000000000 ) ) ;
#16184 = VERTEX_POINT ( 'NONE', #15427 ) ;
#16185 = DIRECTION ( 'NONE',  ( 0.9961946980917461003, -0.04357787137382522491, -0.07547908730516825204 ) ) ;
#16186 = ORIENTED_EDGE ( 'NONE', *, *, #17492, .F. ) ;
#16187 = SURFACE_STYLE_USAGE ( .BOTH. , #16362 ) ;
#16188 = DIRECTION ( 'NONE',  ( 1.000000000000000000, 0.000000000000000000, 0.000000000000000000 ) ) ;
#16189 = DIRECTION ( 'NONE',  ( 0.000000000000000000, 1.387778780781445676E-14, 1.000000000000000000 ) ) ;
#16190 = CARTESIAN_POINT ( 'NONE',  ( -75.21194266656338812, 142.9896906294144969, -20.13387259562454190 ) ) ;
#16191 = B_SPLINE_CURVE_WITH_KNOTS ( 'NONE', 3,
 ( #12033, #13367, #6640, #2744, #12386, #4249, #1500, #10964, #8223, #2828 ),
 .UNSPECIFIED., .F., .F.,
 ( 4, 2, 2, 2, 4 ),
 ( 6.992893892674702526E-18, 0.0003951437508572265816, 0.0007902875017144461159, 0.001185431252571665650, 0.001580575003428885293 ),
 .UNSPECIFIED. ) ;
#16192 = CARTESIAN_POINT ( 'NONE',  ( -19.79962810613638169, 20.00000000000000355, 20.97942696524415851 ) ) ;
#16193 = ORIENTED_EDGE ( 'NONE', *, *, #13896, .T. ) ;
#16194 = DIRECTION ( 'NONE',  ( -2.312964634635742464E-16, 0.000000000000000000, 1.000000000000000000 ) ) ;
#16195 = CARTESIAN_POINT ( 'NONE',  ( -206.8291083847463767, 173.5730938514649324, -4.616715689291535973 ) ) ;
#16196 = DIRECTION ( 'NONE',  ( 1.000000000000000000, 0.000000000000000000, 0.000000000000000000 ) ) ;
#16197 = DIRECTION ( 'NONE',  ( 1.000000000000000000, 0.000000000000000000, -0.000000000000000000 ) ) ;
#16198 = EDGE_CURVE ( 'NONE', #8608, #5246, #11998, .T. ) ;
#16199 = EDGE_CURVE ( 'NONE', #16869, #6523, #4683, .T. ) ;
#16200 = EDGE_CURVE ( 'NONE', #16488, #2665, #6220, .T. ) ;
#16201 = ORIENTED_EDGE ( 'NONE', *, *, #1796, .T. ) ;
#16202 = CARTESIAN_POINT ( 'NONE',  ( -5.000000000000000888, 204.6227766016838245, -2.020667218593133100E-15 ) ) ;
#16203 = ORIENTED_EDGE ( 'NONE', *, *, #2132, .T. ) ;
#16204 = CARTESIAN_POINT ( 'NONE',  ( -75.98251204892453359, 151.0988115558745051, -28.35253695364550097 ) ) ;
#16205 = CARTESIAN_POINT ( 'NONE',  ( -27.99999999999998224, 10.00000000000000000, 11.50215154306610188 ) ) ;
#16206 = EDGE_LOOP ( 'NONE', ( #3461, #1344, #10432, #9439 ) ) ;
#16207 = DIRECTION ( 'NONE',  ( 0.000000000000000000, 0.000000000000000000, -1.000000000000000000 ) ) ;
#16208 = DIRECTION ( 'NONE',  ( 1.000000000000000000, 0.000000000000000000, 0.000000000000000000 ) ) ;
#16209 = CARTESIAN_POINT ( 'NONE',  ( 27.48361012698968864, 138.6227766016838245, 1.063447695028166570E-14 ) ) ;
#16210 = DIRECTION ( 'NONE',  ( -1.000000000000000000, -0.000000000000000000, 0.000000000000000000 ) ) ;
#16211 = LINE ( 'NONE', #5410, #5569 ) ;
#16212 = CARTESIAN_POINT ( 'NONE',  ( 20.21973759693270267, 29.89473369120481294, -11.02800485953945930 ) ) ;
#16213 = DIRECTION ( 'NONE',  ( 8.673617379884036705E-17, -0.000000000000000000, -1.000000000000000000 ) ) ;
#16214 = DIRECTION ( 'NONE',  ( -0.000000000000000000, -0.000000000000000000, 1.000000000000000000 ) ) ;
#16215 = DIRECTION ( 'NONE',  ( 0.000000000000000000, 0.000000000000000000, 1.000000000000000000 ) ) ;
#16216 = SURFACE_SIDE_STYLE ('',( #14961 ) ) ;
#16217 = ORIENTED_EDGE ( 'NONE', *, *, #1758, .T. ) ;
#16218 = DIRECTION ( 'NONE',  ( 0.000000000000000000, -0.8660254037844413721, 0.4999999999999953371 ) ) ;
#16219 = EDGE_CURVE ( 'NONE', #16060, #13616, #7284, .T. ) ;
#16220 = ADVANCED_FACE ( 'NONE', ( #8863 ), #14113, .F. ) ;
#16221 = VERTEX_POINT ( 'NONE', #14720 ) ;
#16222 = FACE_OUTER_BOUND ( 'NONE', #10537, .T. ) ;
#16223 = DIRECTION ( 'NONE',  ( -1.000000000000000000, -0.000000000000000000, -0.000000000000000000 ) ) ;
#16224 = ORIENTED_EDGE ( 'NONE', *, *, #3991, .T. ) ;
#16225 = DIRECTION ( 'NONE',  ( -0.000000000000000000, -0.000000000000000000, -1.000000000000000000 ) ) ;
#16226 = CARTESIAN_POINT ( 'NONE',  ( 15.07980489400154056, 126.2730657262978724, 7.274180996386617970 ) ) ;
#16227 = ORIENTED_EDGE ( 'NONE', *, *, #6019, .T. ) ;
#16228 = CARTESIAN_POINT ( 'NONE',  ( 20.42763382733002686, 19.99999999999999645, 24.23318166603087676 ) ) ;
#16229 = ORIENTED_EDGE ( 'NONE', *, *, #1278, .T. ) ;
#16230 = FACE_OUTER_BOUND ( 'NONE', #10418, .T. ) ;
#16231 = CARTESIAN_POINT ( 'NONE',  ( 36.35693927557340999, 192.6156044230849034, -25.46745035168473947 ) ) ;
#16232 = CARTESIAN_POINT ( 'NONE',  ( 48.00000000000000711, 183.6227766016837961, 5.571800142134975431 ) ) ;
#16233 = DIRECTION ( 'NONE',  ( 0.000000000000000000, 0.8660254037844413721, 0.4999999999999952816 ) ) ;
#16234 = ADVANCED_FACE ( 'NONE', ( #17281 ), #9396, .F. ) ;
#16235 = ORIENTED_EDGE ( 'NONE', *, *, #4147, .T. ) ;
#16236 = CARTESIAN_POINT ( 'NONE',  ( 25.92568854015031121, 149.5391923287904490, 24.52402115671403493 ) ) ;
#16237 = ORIENTED_EDGE ( 'NONE', *, *, #16101, .T. ) ;
#16238 = CARTESIAN_POINT ( 'NONE',  ( -82.00760546193471612, 189.3908747183072592, -27.80828541846620183 ) ) ;
#16239 = DIRECTION ( 'NONE',  ( -1.000000000000000000, 0.000000000000000000, 0.000000000000000000 ) ) ;
#16240 = ORIENTED_EDGE ( 'NONE', *, *, #13000, .F. ) ;
#16241 = ORIENTED_EDGE ( 'NONE', *, *, #12281, .F. ) ;
#16242 = ORIENTED_EDGE ( 'NONE', *, *, #17492, .T. ) ;
#16243 = VECTOR ( 'NONE', #388, 1000.000000000000114 ) ;
#16244 = VECTOR ( 'NONE', #16684, 1000.000000000000000 ) ;
#16245 = LINE ( 'NONE', #10661, #16630 ) ;
#16246 = ORIENTED_EDGE ( 'NONE', *, *, #4473, .T. ) ;
#16247 = DIRECTION ( 'NONE',  ( -1.000000000000000000, 0.000000000000000000, 0.000000000000000000 ) ) ;
#16248 = DIRECTION ( 'NONE',  ( -0.000000000000000000, -1.000000000000000000, -0.000000000000000000 ) ) ;
#16249 = CARTESIAN_POINT ( 'NONE',  ( -96.00000000000001421, 141.6227766016838245, -5.510910596163088767E-15 ) ) ;
#16250 = DIRECTION ( 'NONE',  ( 1.000000000000000000, 0.000000000000000000, 0.000000000000000000 ) ) ;
#16251 = DIRECTION ( 'NONE',  ( 1.000000000000000000, -0.000000000000000000, -0.000000000000000000 ) ) ;
#16252 = CARTESIAN_POINT ( 'NONE',  ( -79.22094317722377355, 151.5769270156786206, 26.21405625665653005 ) ) ;
#16253 = ADVANCED_FACE ( 'NONE', ( #982 ), #2671, .T. ) ;
#16254 = VECTOR ( 'NONE', #16836, 1000.000000000000000 ) ;
#16255 = ORIENTED_EDGE ( 'NONE', *, *, #17387, .T. ) ;
#16256 = CARTESIAN_POINT ( 'NONE',  ( -85.83427352782426567, 198.0686797691926415, -22.93241811017416154 ) ) ;
#16257 = DIRECTION ( 'NONE',  ( -0.000000000000000000, -0.000000000000000000, -1.000000000000000000 ) ) ;
#16258 = DIRECTION ( 'NONE',  ( -1.000000000000000000, 0.000000000000000000, 0.000000000000000000 ) ) ;
#16259 = CARTESIAN_POINT ( 'NONE',  ( -207.4350753193408252, 173.4018121924175944, 4.916187366912743606 ) ) ;
#16260 = DIRECTION ( 'NONE',  ( -8.673617379884036705E-17, 0.000000000000000000, 1.000000000000000000 ) ) ;
#16261 = EDGE_CURVE ( 'NONE', #102, #10869, #1535, .T. ) ;
#16262 = EDGE_CURVE ( 'NONE', #17055, #5035, #10542, .T. ) ;
#16263 = DIRECTION ( 'NONE',  ( -0.8660254037844378194, -0.5000000000000015543, -0.000000000000000000 ) ) ;
#16264 = ORIENTED_EDGE ( 'NONE', *, *, #11617, .T. ) ;
#16265 = CARTESIAN_POINT ( 'NONE',  ( -70.00000000000000000, 171.6227766016838245, 0.000000000000000000 ) ) ;
#16266 = VECTOR ( 'NONE', #5954, 1000.000000000000000 ) ;
#16267 = VERTEX_POINT ( 'NONE', #1079 ) ;
#16268 = DIRECTION ( 'NONE',  ( 0.000000000000000000, 1.734723475976807094E-15, 1.000000000000000000 ) ) ;
#16269 =( GEOMETRIC_REPRESENTATION_CONTEXT ( 3 ) GLOBAL_UNCERTAINTY_ASSIGNED_CONTEXT ( ( #9147 ) ) GLOBAL_UNIT_ASSIGNED_CONTEXT ( ( #2199, #10253, #4692 ) ) REPRESENTATION_CONTEXT ( 'NONE', 'WORKASPACE' ) );
#16270 = DIRECTION ( 'NONE',  ( -1.000000000000000000, -0.000000000000000000, -0.000000000000000000 ) ) ;
#16271 = DIRECTION ( 'NONE',  ( 8.673617379884037937E-17, 0.000000000000000000, 1.000000000000000000 ) ) ;
#16272 = CARTESIAN_POINT ( 'NONE',  ( 2.370000000000000551, 0.000000000000000000, 0.000000000000000000 ) ) ;
#16273 = VERTEX_POINT ( 'NONE', #7895 ) ;
#16274 = CARTESIAN_POINT ( 'NONE',  ( -48.00000000000000000, 154.3022685259950038, 9.999999999999900524 ) ) ;
#16275 = DIRECTION ( 'NONE',  ( 0.000000000000000000, -0.8660254037844413721, -0.4999999999999953371 ) ) ;
#16276 = DIRECTION ( 'NONE',  ( -0.000000000000000000, -0.000000000000000000, 1.000000000000000000 ) ) ;
#16277 = LINE ( 'NONE', #9536, #10602 ) ;
#16278 = MECHANICAL_DESIGN_GEOMETRIC_PRESENTATION_REPRESENTATION (  '', ( #2413 ), #4954 ) ;
#16279 = AXIS2_PLACEMENT_3D ( 'NONE', #8277, #11192, #13686 ) ;
#16280 = VECTOR ( 'NONE', #16628, 1000.000000000000000 ) ;
#16281 = CARTESIAN_POINT ( 'NONE',  ( 15.33542211484438056, 137.4551579351490318, -9.454295640945616697 ) ) ;
#16282 = VERTEX_POINT ( 'NONE', #11963 ) ;
#16283 = DIRECTION ( 'NONE',  ( 0.000000000000000000, 0.000000000000000000, 1.000000000000000000 ) ) ;
#16284 = LINE ( 'NONE', #2826, #12317 ) ;
#16285 = VERTEX_POINT ( 'NONE', #15866 ) ;
#16286 = DIRECTION ( 'NONE',  ( -1.000000000000000000, -0.000000000000000000, -0.000000000000000000 ) ) ;
#16287 = CLOSED_SHELL ( 'NONE', ( #17059, #6888, #4896, #11168, #14039, #9752 ) ) ;
#16288 = CIRCLE ( 'NONE', #1008, 10.00000000000000178 ) ;
#16289 = DIRECTION ( 'NONE',  ( -0.000000000000000000, -0.8660254037844363761, -0.5000000000000039968 ) ) ;
#16290 = EDGE_CURVE ( 'NONE', #14342, #209, #15948, .T. ) ;
#16291 = CIRCLE ( 'NONE', #15722, 2.500000000000002220 ) ;
#16292 = CARTESIAN_POINT ( 'NONE',  ( 27.43384137083016583, 192.3153571870206235, 25.70724251753713929 ) ) ;
#16293 = CARTESIAN_POINT ( 'NONE',  ( 34.93420767853314146, 18.00000000000000355, -6.320602137672510779 ) ) ;
#16294 = CARTESIAN_POINT ( 'NONE',  ( 17.77234289100693232, 17.99999999999999289, -12.54415977683811256 ) ) ;
#16295 = DIRECTION ( 'NONE',  ( 1.000000000000000000, -0.000000000000000000, -0.000000000000000000 ) ) ;
#16296 = DIRECTION ( 'NONE',  ( -1.156482317317868274E-16, 1.000000000000000000, 0.000000000000000000 ) ) ;
#16297 = DIRECTION ( 'NONE',  ( 1.000000000000000000, 0.000000000000000000, -0.000000000000000000 ) ) ;
#16298 = FILL_AREA_STYLE ('',( #9556 ) ) ;
#16299 = B_SPLINE_CURVE_WITH_KNOTS ( 'NONE', 3,
 ( #13098, #3797, #10608, #15846, #6636, #9376, #16119, #14693, #14778, #9193, #7868, #10433, #14598, #2474, #2573, #5308, #9020, #13363, #13279, #7960, #3720, #1146, #16017, #6549, #12029, #2650, #8041, #13449, #1320, #11940, #17342, #14434, #2298, #964, #16465, #16204, #13710, #12473, #12125, #340, #8130, #5479, #1676, #13631 ),
 .UNSPECIFIED., .F., .F.,
 ( 4, 2, 2, 2, 2, 2, 2, 2, 2, 2, 2, 2, 2, 2, 2, 2, 2, 2, 2, 2, 2, 4 ),
 ( 0.02539562174428233732, 0.02674754696500270326, 0.02742350957536288450, 0.02809947218572306574, 0.02945139740644348719, 0.03012736001680369619, 0.03080332262716390171, 0.03215524784788428847, 0.03283121045824447665, 0.03350717306860466482, 0.03418313567896484606, 0.03485909828932503424, 0.03621102351004540365, 0.03688698612040561264, 0.03756294873076582164, 0.03891487395148625350, 0.03959083656184648331, 0.04026679917220671312, 0.04161872439292722825, 0.04297064961364774338, 0.04432257483436825851, 0.04702642527580928183 ),
 .UNSPECIFIED. ) ;
#16300 = VERTEX_POINT ( 'NONE', #14529 ) ;
#16301 = CARTESIAN_POINT ( 'NONE',  ( 27.99999999999998224, 9.999999999999998224, -30.00000000000001066 ) ) ;
#16302 = ORIENTED_EDGE ( 'NONE', *, *, #3440, .F. ) ;
#16303 = CYLINDRICAL_SURFACE ( 'NONE', #8343, 2.500000000000000444 ) ;
#16304 = AXIS2_PLACEMENT_3D ( 'NONE', #9990, #12757, #3191 ) ;
#16305 = AXIS2_PLACEMENT_3D ( 'NONE', #16754, #15410, #4705 ) ;
#16306 = CARTESIAN_POINT ( 'NONE',  ( 2.370000000000000551, 0.000000000000000000, 4.750000000000000000 ) ) ;
#16307 = AXIS2_PLACEMENT_3D ( 'NONE', #9456, #16025, #9382 ) ;
#16308 = ORIENTED_EDGE ( 'NONE', *, *, #6752, .F. ) ;
#16309 = CARTESIAN_POINT ( 'NONE',  ( 15.00000000000000000, 204.6227766016838245, 2.020667218593133100E-15 ) ) ;
#16310 = AXIS2_PLACEMENT_3D ( 'NONE', #7356, #4789, #7264 ) ;
#16311 = CARTESIAN_POINT ( 'NONE',  ( -5.000000000000004441, 144.1839557653416080, -18.33333333333336057 ) ) ;
#16312 = ORIENTED_EDGE ( 'NONE', *, *, #3605, .F. ) ;
#16313 = CARTESIAN_POINT ( 'NONE',  ( 29.43652167955699994, 154.1240291517870276, -27.97845313684488033 ) ) ;
#16314 = EDGE_LOOP ( 'NONE', ( #996, #959, #1821, #45 ) ) ;
#16315 = ADVANCED_FACE ( 'NONE', ( #5236 ), #9152, .F. ) ;
#16316 = ADVANCED_FACE ( 'NONE', ( #8242 ), #100, .T. ) ;
#16317 = ADVANCED_FACE ( 'NONE', ( #1607 ), #4346, .F. ) ;
#16318 = DIRECTION ( 'NONE',  ( 1.000000000000000000, -0.000000000000000000, -0.000000000000000000 ) ) ;
#16319 = AXIS2_PLACEMENT_3D ( 'NONE', #4165, #4255, #10801 ) ;
#16320 = FACE_OUTER_BOUND ( 'NONE', #2159, .T. ) ;
#16321 = CARTESIAN_POINT ( 'NONE',  ( -102.0000000000000142, 171.6227766016838245, 28.26633746182137585 ) ) ;
#16322 = EDGE_LOOP ( 'NONE', ( #9306, #11485, #5543, #4193 ) ) ;
#16323 = VECTOR ( 'NONE', #9007, 1000.000000000000000 ) ;
#16324 = FACE_OUTER_BOUND ( 'NONE', #5758, .T. ) ;
#16325 =( GEOMETRIC_REPRESENTATION_CONTEXT ( 3 ) GLOBAL_UNCERTAINTY_ASSIGNED_CONTEXT ( ( #10185 ) ) GLOBAL_UNIT_ASSIGNED_CONTEXT ( ( #8373, #13792, #4401 ) ) REPRESENTATION_CONTEXT ( 'NONE', 'WORKASPACE' ) );
#16326 = VECTOR ( 'NONE', #3630, 1000.000000000000000 ) ;
#16327 = ORIENTED_EDGE ( 'NONE', *, *, #9482, .T. ) ;
#16328 = CARTESIAN_POINT ( 'NONE',  ( 27.42854581659407742, 150.9146311475675759, 25.69413650784048642 ) ) ;
#16329 = VERTEX_POINT ( 'NONE', #6838 ) ;
#16330 = CARTESIAN_POINT ( 'NONE',  ( -208.1430079281944074, 176.3671987152221448, -3.647967993167786194 ) ) ;
#16331 = DIRECTION ( 'NONE',  ( 1.000000000000000000, -0.000000000000000000, -0.000000000000000000 ) ) ;
#16332 = DIRECTION ( 'NONE',  ( -1.000000000000000000, 0.000000000000000000, 0.000000000000000000 ) ) ;
#16333 = EDGE_LOOP ( 'NONE', ( #9408, #1085, #14795, #11257 ) ) ;
#16334 = ORIENTED_EDGE ( 'NONE', *, *, #15961, .T. ) ;
#16335 = VECTOR ( 'NONE', #1051, 1000.000000000000000 ) ;
#16336 = CIRCLE ( 'NONE', #1054, 2.500000000000000444 ) ;
#16337 = CARTESIAN_POINT ( 'NONE',  ( 10.45945364060320237, 139.0001874602887995, 13.88305366436938115 ) ) ;
#16338 = AXIS2_PLACEMENT_3D ( 'NONE', #8998, #6336, #1209 ) ;
#16339 = VERTEX_POINT ( 'NONE', #16309 ) ;
#16340 = PRODUCT_CONTEXT ( 'NONE', #1332, 'mechanical' ) ;
#16341 = DIRECTION ( 'NONE',  ( -1.000000000000000000, 0.000000000000000000, 0.000000000000000000 ) ) ;
#16342 = DIRECTION ( 'NONE',  ( -1.156482317317868274E-16, 1.000000000000000000, 0.000000000000000000 ) ) ;
#16343 = CARTESIAN_POINT ( 'NONE',  ( -23.00000000000000000, 122.0000000000000284, 0.000000000000000000 ) ) ;
#16344 = FACE_OUTER_BOUND ( 'NONE', #7689, .T. ) ;
#16345 = LINE ( 'NONE', #12260, #5536 ) ;
#16346 = PRODUCT_DEFINITION_SHAPE ( 'NONE', 'NONE',  #17347 ) ;
#16347 = ORIENTED_EDGE ( 'NONE', *, *, #16638, .F. ) ;
#16348 = CARTESIAN_POINT ( 'NONE',  ( -77.58098289114030877, 202.1180966153993097, -17.17743398583135672 ) ) ;
#16349 = CIRCLE ( 'NONE', #5021, 27.69059892324149175 ) ;
#16350 = CARTESIAN_POINT ( 'NONE',  ( 13.59940502541562246, 130.1762661646492063, 12.36432683418100353 ) ) ;
#16351 = CARTESIAN_POINT ( 'NONE',  ( 34.93420767853316988, 20.00000000000000000, -4.999999999999999112 ) ) ;
#16352 = DIRECTION ( 'NONE',  ( 1.000000000000000000, 0.000000000000000000, 0.000000000000000000 ) ) ;
#16353 = CARTESIAN_POINT ( 'NONE',  ( -100.0000000000000000, 171.6227766016838245, 27.69059892324149175 ) ) ;
#16354 = AXIS2_PLACEMENT_3D ( 'NONE', #9109, #6731, #1060 ) ;
#16355 = VERTEX_POINT ( 'NONE', #12403 ) ;
#16356 = DIRECTION ( 'NONE',  ( 0.000000000000000000, 0.000000000000000000, 1.000000000000000000 ) ) ;
#16357 = ADVANCED_FACE ( 'NONE', ( #5682 ), #11069, .T. ) ;
#16358 = ORIENTED_EDGE ( 'NONE', *, *, #14204, .F. ) ;
#16359 = EDGE_CURVE ( 'NONE', #16418, #5242, #11142, .T. ) ;
#16360 =( LENGTH_UNIT ( ) NAMED_UNIT ( * ) SI_UNIT ( .MILLI., .METRE. ) );
#16361 = EDGE_LOOP ( 'NONE', ( #8251, #14904 ) ) ;
#16362 = SURFACE_SIDE_STYLE ('',( #3779 ) ) ;
#16363 = VECTOR ( 'NONE', #1811, 1000.000000000000114 ) ;
#16364 = CARTESIAN_POINT ( 'NONE',  ( -91.33974596215564645, 171.6227766016838245, 0.000000000000000000 ) ) ;
#16365 = AXIS2_PLACEMENT_3D ( 'NONE', #1726, #9029, #8533 ) ;
#16366 = CARTESIAN_POINT ( 'NONE',  ( 0.000000000000000000, 20.00000000000000000, 0.000000000000000000 ) ) ;
#16367 = CARTESIAN_POINT ( 'NONE',  ( -206.6025269363104826, 166.6884528440272106, 0.5648560453502019518 ) ) ;
#16368 = EDGE_CURVE ( 'NONE', #8608, #10629, #15669, .T. ) ;
#16369 = ORIENTED_EDGE ( 'NONE', *, *, #4762, .F. ) ;
#16370 = DIRECTION ( 'NONE',  ( -1.000000000000000000, 0.000000000000000000, 0.000000000000000000 ) ) ;
#16371 = CARTESIAN_POINT ( 'NONE',  ( -70.00000000000000000, 154.3022685259950038, -9.999999999999900524 ) ) ;
#16372 = CYLINDRICAL_SURFACE ( 'NONE', #11038, 5.000000000000018652 ) ;
#16373 = DIRECTION ( 'NONE',  ( -0.000000000000000000, -0.000000000000000000, 1.000000000000000000 ) ) ;
#16374 = VECTOR ( 'NONE', #2541, 1000.000000000000000 ) ;
#16375 = AXIS2_PLACEMENT_3D ( 'NONE', #877, #3523, #8911 ) ;
#16376 = CARTESIAN_POINT ( 'NONE',  ( 16.30283403932978459, 136.8379281265527254, -4.993081733805620814 ) ) ;
#16377 = ORIENTED_EDGE ( 'NONE', *, *, #14565, .F. ) ;
#16378 = EDGE_CURVE ( 'NONE', #3275, #15090, #11147, .T. ) ;
#16379 = DIRECTION ( 'NONE',  ( 0.000000000000000000, 1.000000000000000000, 0.000000000000000000 ) ) ;
#16380 = DIRECTION ( 'NONE',  ( 1.000000000000000000, 0.000000000000000000, 0.000000000000000000 ) ) ;
#16381 = EDGE_LOOP ( 'NONE', ( #438, #1182, #6674, #15058 ) ) ;
#16382 =( NAMED_UNIT ( * ) PLANE_ANGLE_UNIT ( ) SI_UNIT ( $, .RADIAN. ) );
#16383 = CARTESIAN_POINT ( 'NONE',  ( 2.749999999999999112, 0.000000000000000000, 0.000000000000000000 ) ) ;
#16384 = DIRECTION ( 'NONE',  ( 0.000000000000000000, 0.000000000000000000, 1.000000000000000000 ) ) ;
#16385 = CIRCLE ( 'NONE', #15234, 2.500000000000000000 ) ;
#16386 = ADVANCED_FACE ( 'NONE', ( #11670 ), #9992, .F. ) ;
#16387 = VECTOR ( 'NONE', #584, 1000.000000000000000 ) ;
#16388 = FACE_OUTER_BOUND ( 'NONE', #12357, .T. ) ;
#16389 = EDGE_CURVE ( 'NONE', #13669, #8380, #158, .T. ) ;
#16390 = VECTOR ( 'NONE', #8327, 1000.000000000000000 ) ;
#16391 = DIRECTION ( 'NONE',  ( -1.000000000000000000, -0.000000000000000000, -0.000000000000000000 ) ) ;
#16392 = EDGE_CURVE ( 'NONE', #7907, #14433, #4162, .T. ) ;
#16393 = CARTESIAN_POINT ( 'NONE',  ( -45.00000000000000000, 134.2062027339443944, -15.00000000000000000 ) ) ;
#16394 = CARTESIAN_POINT ( 'NONE',  ( 14.29542716350633214, 143.4273548044023698, -17.14909632368674508 ) ) ;
#16395 = FILL_AREA_STYLE_COLOUR ( '', #3256 ) ;
#16396 = EDGE_LOOP ( 'NONE', ( #1499, #1624 ) ) ;
#16397 = CARTESIAN_POINT ( 'NONE',  ( -3.000000000000000888, 154.3022685259950038, 9.999999999999900524 ) ) ;
#16398 = EDGE_LOOP ( 'NONE', ( #9478, #8153, #6685, #8952 ) ) ;
#16399 = CARTESIAN_POINT ( 'NONE',  ( 24.99836435517920918, 19.99999999999999289, -6.327826241642252825 ) ) ;
#16400 = AXIS2_PLACEMENT_3D ( 'NONE', #13442, #6812, #7761 ) ;
#16401 = CARTESIAN_POINT ( 'NONE',  ( 15.00000000000000000, 143.0344144757318929, -16.50549856913627877 ) ) ;
#16402 = ADVANCED_FACE ( 'NONE', ( #892 ), #2118, .T. ) ;
#16403 = EDGE_LOOP ( 'NONE', ( #14769, #1453, #480, #4021 ) ) ;
#16404 = CARTESIAN_POINT ( 'NONE',  ( -17.89548297089572060, 32.23709896788771090, 7.636891392351368602 ) ) ;
#16405 = AXIS2_PLACEMENT_3D ( 'NONE', #3777, #17237, #11919 ) ;
#16406 = DIRECTION ( 'NONE',  ( -0.000000000000000000, -0.000000000000000000, 1.000000000000000000 ) ) ;
#16407 = VERTEX_POINT ( 'NONE', #8587 ) ;
#16408 = CARTESIAN_POINT ( 'NONE',  ( 37.50000000000000711, 146.6227766016838245, -21.54065922853802562 ) ) ;
#16409 = ORIENTED_EDGE ( 'NONE', *, *, #5277, .T. ) ;
#16410 = DIRECTION ( 'NONE',  ( -1.000000000000000000, 0.000000000000000000, 0.000000000000000000 ) ) ;
#16411 = CARTESIAN_POINT ( 'NONE',  ( 17.00000000000000000, 171.6227766016838245, 0.000000000000000000 ) ) ;
#16412 = AXIS2_PLACEMENT_3D ( 'NONE', #691, #9974, #6085 ) ;
#16413 = VECTOR ( 'NONE', #3788, 1000.000000000000000 ) ;
#16414 = DIRECTION ( 'NONE',  ( 0.000000000000000000, -0.4999999999999952816, -0.8660254037844413721 ) ) ;
#16415 = ORIENTED_EDGE ( 'NONE', *, *, #5030, .T. ) ;
#16416 = PLANE ( 'NONE',  #11705 ) ;
#16417 = VECTOR ( 'NONE', #5313, 1000.000000000000000 ) ;
#16418 = VERTEX_POINT ( 'NONE', #10260 ) ;
#16419 = CARTESIAN_POINT ( 'NONE',  ( 19.49215236471922807, 140.4173771131980857, -15.85404464849102268 ) ) ;
#16420 = ORIENTED_EDGE ( 'NONE', *, *, #12512, .T. ) ;
#16421 = CARTESIAN_POINT ( 'NONE',  ( -77.73879888791972803, 189.4484344766680977, -27.77174765869276030 ) ) ;
#16422 = DIRECTION ( 'NONE',  ( 0.000000000000000000, 0.000000000000000000, 1.000000000000000000 ) ) ;
#16423 = SHAPE_REPRESENTATION ( 'Left Housing Shell', ( #3583 ), #11517 ) ;
#16424 = ADVANCED_FACE ( 'NONE', ( #14181 ), #12914, .F. ) ;
#16425 = DIRECTION ( 'NONE',  ( 0.000000000000000000, 0.000000000000000000, -1.000000000000000000 ) ) ;
#16426 = ADVANCED_FACE ( 'NONE', ( #15494, #2042 ), #17003, .F. ) ;
#16427 = VERTEX_POINT ( 'NONE', #11340 ) ;
#16428 = EDGE_CURVE ( 'NONE', #3610, #5121, #6411, .T. ) ;
#16429 = ORIENTED_EDGE ( 'NONE', *, *, #2079, .T. ) ;
#16430 = DIRECTION ( 'NONE',  ( -0.000000000000000000, -0.000000000000000000, -1.000000000000000000 ) ) ;
#16431 = CARTESIAN_POINT ( 'NONE',  ( -72.56315672547016504, 197.7246901893026347, -20.20962120078075586 ) ) ;
#16432 = DIRECTION ( 'NONE',  ( -1.000000000000000000, 0.000000000000000000, 0.000000000000000000 ) ) ;
#16433 = AXIS2_PLACEMENT_3D ( 'NONE', #5529, #11014, #7035 ) ;
#16434 = ORIENTED_EDGE ( 'NONE', *, *, #2970, .T. ) ;
#16435 = DIRECTION ( 'NONE',  ( -1.000000000000000000, 0.000000000000000000, 0.000000000000000000 ) ) ;
#16436 = CARTESIAN_POINT ( 'NONE',  ( -68.00000000000000000, 171.6227766016838245, -2.602085213965210642E-15 ) ) ;
#16437 = CARTESIAN_POINT ( 'NONE',  ( 15.00000000000000000, 191.6227766016837961, 1.224646799147353454E-15 ) ) ;
#16438 = CARTESIAN_POINT ( 'NONE',  ( 40.00000000000000711, 0.000000000000000000, 0.000000000000000000 ) ) ;
#16439 = CARTESIAN_POINT ( 'NONE',  ( -5.000000000000000888, 171.6227766016838245, 0.000000000000000000 ) ) ;
#16440 = CARTESIAN_POINT ( 'NONE',  ( 18.97220464449422295, 17.99999999999999645, 12.00279687791388383 ) ) ;
#16441 = ORIENTED_EDGE ( 'NONE', *, *, #10016, .T. ) ;
#16442 = CARTESIAN_POINT ( 'NONE',  ( -81.28398610579327510, 202.4851391218124945, -16.50809708901795148 ) ) ;
#16443 = CARTESIAN_POINT ( 'NONE',  ( 196.0000000000000000, 191.6227766016837677, -5.571800142134975431 ) ) ;
#16444 = CARTESIAN_POINT ( 'NONE',  ( -20.85786437626906675, 124.1421356237309652, 14.99999999999998401 ) ) ;
#16445 = LINE ( 'NONE', #14756, #10971 ) ;
#16446 = FACE_OUTER_BOUND ( 'NONE', #7168, .T. ) ;
#16447 = ORIENTED_EDGE ( 'NONE', *, *, #5475, .T. ) ;
#16448 = ADVANCED_FACE ( 'NONE', ( #7435 ), #3193, .T. ) ;
#16449 = EDGE_CURVE ( 'NONE', #11802, #10963, #15401, .T. ) ;
#16450 = CARTESIAN_POINT ( 'NONE',  ( -68.00000000000000000, 171.6227766016838245, 0.000000000000000000 ) ) ;
#16451 = ORIENTED_EDGE ( 'NONE', *, *, #15693, .F. ) ;
#16452 = DIRECTION ( 'NONE',  ( -1.000000000000000000, -0.000000000000000000, -0.000000000000000000 ) ) ;
#16453 = CIRCLE ( 'NONE', #10776, 8.000000000000000000 ) ;
#16454 = ORIENTED_EDGE ( 'NONE', *, *, #16392, .T. ) ;
#16455 = DIRECTION ( 'NONE',  ( 0.000000000000000000, 0.000000000000000000, -1.000000000000000000 ) ) ;
#16456 = DIRECTION ( 'NONE',  ( 7.523163845262643335E-32, -1.000000000000000000, -8.673617379884037444E-16 ) ) ;
#16457 = ORIENTED_EDGE ( 'NONE', *, *, #5640, .F. ) ;
#16458 = LINE ( 'NONE', #14846, #17468 ) ;
#16459 = CARTESIAN_POINT ( 'NONE',  ( -68.00000000000000000, 171.6227766016838245, -25.00000000000000000 ) ) ;
#16460 = FACE_BOUND ( 'NONE', #6859, .T. ) ;
#16461 = EDGE_CURVE ( 'NONE', #4201, #6776, #11414, .T. ) ;
#16462 = DIRECTION ( 'NONE',  ( -1.000000000000000000, -0.000000000000000000, -0.000000000000000000 ) ) ;
#16463 = CARTESIAN_POINT ( 'NONE',  ( 13.38958197704232056, 130.3612470323695902, -12.52688079436099144 ) ) ;
#16464 = ORIENTED_EDGE ( 'NONE', *, *, #10670, .T. ) ;
#16465 = CARTESIAN_POINT ( 'NONE',  ( -76.47766082881949501, 151.4845562501469942, -28.62650789566041709 ) ) ;
#16466 = DIRECTION ( 'NONE',  ( 0.000000000000000000, 0.000000000000000000, 1.000000000000000000 ) ) ;
#16467 = ORIENTED_EDGE ( 'NONE', *, *, #61, .F. ) ;
#16468 = SURFACE_SIDE_STYLE ('',( #5662 ) ) ;
#16469 = CARTESIAN_POINT ( 'NONE',  ( -50.00000000000000000, 143.0439382767972631, 16.49999999999984013 ) ) ;
#16470 = FACE_OUTER_BOUND ( 'NONE', #10751, .T. ) ;
#16471 = CARTESIAN_POINT ( 'NONE',  ( 28.10980041848796063, 191.9899036175949618, 25.96511099662696509 ) ) ;
#16472 = DIRECTION ( 'NONE',  ( -0.000000000000000000, -0.000000000000000000, 1.000000000000000000 ) ) ;
#16473 = CARTESIAN_POINT ( 'NONE',  ( 1.559999999999998943, 0.8660254037844428154, -1.499999999999997780 ) ) ;
#16474 = CYLINDRICAL_SURFACE ( 'NONE', #3939, 2.500000000000000444 ) ;
#16475 = DIRECTION ( 'NONE',  ( 0.000000000000000000, -0.000000000000000000, 1.000000000000000000 ) ) ;
#16476 = ADVANCED_FACE ( 'NONE', ( #12836 ), #7516, .T. ) ;
#16477 = PRESENTATION_STYLE_ASSIGNMENT (( #534 ) ) ;
#16478 = ORIENTED_EDGE ( 'NONE', *, *, #9014, .T. ) ;
#16479 = EDGE_LOOP ( 'NONE', ( #1924, #13326, #7647, #11714 ) ) ;
#16480 = CARTESIAN_POINT ( 'NONE',  ( 23.06881488990584472, 29.89244155294396066, -10.82591622123929653 ) ) ;
#16481 = PRODUCT_RELATED_PRODUCT_CATEGORY ( 'part', '', ( #4183 ) ) ;
#16482 = CARTESIAN_POINT ( 'NONE',  ( 34.93420767853316988, 30.00000000000000000, -15.00000000000000000 ) ) ;
#16483 = ORIENTED_EDGE ( 'NONE', *, *, #16038, .T. ) ;
#16484 = ADVANCED_FACE ( 'NONE', ( #16826 ), #4698, .F. ) ;
#16485 = DIRECTION ( 'NONE',  ( 0.000000000000000000, 0.000000000000000000, -1.000000000000000000 ) ) ;
#16486 = ADVANCED_FACE ( 'NONE', ( #6025 ), #10180, .T. ) ;
#16487 = LINE ( 'NONE', #4535, #8207 ) ;
#16488 = VERTEX_POINT ( 'NONE', #15582 ) ;
#16489 = CARTESIAN_POINT ( 'NONE',  ( 35.93543503013834339, 151.2142461003564335, -25.93356563065114528 ) ) ;
#16490 = CARTESIAN_POINT ( 'NONE',  ( -72.50000000000002842, 146.6227766016838245, -21.54065922853802562 ) ) ;
#16491 = LINE ( 'NONE', #3548, #6970 ) ;
#16492 = CARTESIAN_POINT ( 'NONE',  ( 40.00000000000000000, 20.00000000000000000, 0.000000000000000000 ) ) ;
#16493 = CARTESIAN_POINT ( 'NONE',  ( 17.00000000000000000, 171.6227766016838245, 0.000000000000000000 ) ) ;
#16494 = DIRECTION ( 'NONE',  ( 0.000000000000000000, -0.4999999999999952816, 0.8660254037844413721 ) ) ;
#16495 = LINE ( 'NONE', #13845, #2679 ) ;
#16496 = ORIENTED_EDGE ( 'NONE', *, *, #14562, .F. ) ;
#16497 = DIRECTION ( 'NONE',  ( 1.000000000000000000, 0.000000000000000000, 0.000000000000000000 ) ) ;
#16498 = ORIENTED_EDGE ( 'NONE', *, *, #16889, .T. ) ;
#16499 = CARTESIAN_POINT ( 'NONE',  ( -22.99999999999999289, 90.00000000000000000, -15.00000000000000000 ) ) ;
#16500 = PLANE ( 'NONE',  #2743 ) ;
#16501 = DIRECTION ( 'NONE',  ( 1.000000000000000000, 0.000000000000000000, 0.000000000000000000 ) ) ;
#16502 = ORIENTED_EDGE ( 'NONE', *, *, #12951, .F. ) ;
#16503 = ORIENTED_EDGE ( 'NONE', *, *, #2529, .F. ) ;
#16504 = DIRECTION ( 'NONE',  ( 0.000000000000000000, 0.000000000000000000, 1.000000000000000000 ) ) ;
#16505 = DIRECTION ( 'NONE',  ( -1.000000000000000000, 0.000000000000000000, 0.000000000000000000 ) ) ;
#16506 = CARTESIAN_POINT ( 'NONE',  ( 16.30283403932918063, 136.8379281265527254, 4.993081733805470712 ) ) ;
#16507 = EDGE_LOOP ( 'NONE', ( #13402, #12623, #7605, #7618, #7512 ) ) ;
#16508 = ITEM_DEFINED_TRANSFORMATION ( 'NONE', 'NONE', #6139,  #3583 ) ;
#16509 = CARTESIAN_POINT ( 'NONE',  ( -27.99999999999998224, 10.00000000000000000, 1.387778780781445676E-14 ) ) ;
#16510 = LINE ( 'NONE', #12438, #10327 ) ;
#16511 = CARTESIAN_POINT ( 'NONE',  ( -80.00000000000002842, 146.6227766016838245, -13.00000000000000000 ) ) ;
#16512 = CARTESIAN_POINT ( 'NONE',  ( 27.44407568426044008, 138.8271129316868837, 3.666666666666658081 ) ) ;
#16513 = ADVANCED_FACE ( 'NONE', ( #3459 ), #3542, .F. ) ;
#16514 = CARTESIAN_POINT ( 'NONE',  ( 18.26135686777217160, 17.99999999999999289, 12.35203162874035065 ) ) ;
#16515 = ORIENTED_EDGE ( 'NONE', *, *, #937, .F. ) ;
#16516 = CARTESIAN_POINT ( 'NONE',  ( -75.00711853871067092, 199.9683764595549178, -20.53727899274374025 ) ) ;
#16517 = FACE_OUTER_BOUND ( 'NONE', #11749, .T. ) ;
#16518 = CARTESIAN_POINT ( 'NONE',  ( 22.61491075001043782, 19.99999999999999645, -23.50024419593056635 ) ) ;
#16519 = DIRECTION ( 'NONE',  ( 0.000000000000000000, 0.000000000000000000, -1.000000000000000000 ) ) ;
#16520 = DIRECTION ( 'NONE',  ( -1.000000000000000000, -6.938893903907228378E-16, 0.000000000000000000 ) ) ;
#16521 = AXIS2_PLACEMENT_3D ( 'NONE', #15309, #3183, #6989 ) ;
#16522 = ORIENTED_EDGE ( 'NONE', *, *, #3173, .T. ) ;
#16523 = VERTEX_POINT ( 'NONE', #17433 ) ;
#16524 = CARTESIAN_POINT ( 'NONE',  ( 6.714477151836450552, 134.0780154003031726, 13.00000000000000000 ) ) ;
#16525 = ORIENTED_EDGE ( 'NONE', *, *, #8981, .F. ) ;
#16526 = CARTESIAN_POINT ( 'NONE',  ( 27.50000000000001066, 146.6227766016838245, 10.00000000000000178 ) ) ;
#16527 = EDGE_LOOP ( 'NONE', ( #1558, #2971, #12371, #10135 ) ) ;
#16528 = SURFACE_STYLE_USAGE ( .BOTH. , #1562 ) ;
#16529 = DIRECTION ( 'NONE',  ( 0.000000000000000000, 0.000000000000000000, 1.000000000000000000 ) ) ;
#16530 = CARTESIAN_POINT ( 'NONE',  ( -5.000000000000004441, 134.2062027339443944, -25.00000000000000000 ) ) ;
#16531 = VECTOR ( 'NONE', #3383, 1000.000000000000000 ) ;
#16532 = DIRECTION ( 'NONE',  ( 0.000000000000000000, 1.000000000000000000, -1.224646799147353207E-16 ) ) ;
#16533 = ADVANCED_FACE ( 'NONE', ( #3898, #5212 ), #15925, .T. ) ;
#16534 = EDGE_CURVE ( 'NONE', #15849, #2797, #10703, .T. ) ;
#16535 = LINE ( 'NONE', #503, #4406 ) ;
#16536 = AXIS2_PLACEMENT_3D ( 'NONE', #13648, #9564, #7173 ) ;
#16537 = EDGE_CURVE ( 'NONE', #570, #14499, #7771, .T. ) ;
#16538 = EDGE_CURVE ( 'NONE', #3758, #11751, #5134, .T. ) ;
#16539 = VERTEX_POINT ( 'NONE', #17257 ) ;
#16540 = CARTESIAN_POINT ( 'NONE',  ( 32.22389789336222776, 142.1412512070565413, 14.82809033015228195 ) ) ;
#16541 = CARTESIAN_POINT ( 'NONE',  ( -43.00000000000000000, 134.2062027339443944, 25.00000000000000000 ) ) ;
#16542 = DIRECTION ( 'NONE',  ( -1.000000000000000000, -0.000000000000000000, -0.000000000000000000 ) ) ;
#16543 = FACE_OUTER_BOUND ( 'NONE', #10065, .T. ) ;
#16544 = CARTESIAN_POINT ( 'NONE',  ( 17.03671980602049985, 126.4628225884666932, -7.681944018317823364 ) ) ;
#16545 = VECTOR ( 'NONE', #17222, 1000.000000000000000 ) ;
#16546 = VERTEX_POINT ( 'NONE', #6727 ) ;
#16547 = DIRECTION ( 'NONE',  ( -1.000000000000000000, 0.000000000000000000, 0.000000000000000000 ) ) ;
#16548 = ORIENTED_EDGE ( 'NONE', *, *, #10692, .F. ) ;
#16549 =( LENGTH_UNIT ( ) NAMED_UNIT ( * ) SI_UNIT ( .MILLI., .METRE. ) );
#16550 = CARTESIAN_POINT ( 'NONE',  ( -85.13898110008898357, 193.5203449394525137, -27.30457132278912624 ) ) ;
#16551 = EDGE_CURVE ( 'NONE', #6848, #11049, #11849, .T. ) ;
#16552 = DIRECTION ( 'NONE',  ( -1.000000000000000000, 2.707861035671114735E-15, 0.000000000000000000 ) ) ;
#16553 = CARTESIAN_POINT ( 'NONE',  ( 25.46628596442746684, 194.4926179048318602, 23.79294127240566681 ) ) ;
#16554 = LINE ( 'NONE', #16813, #9728 ) ;
#16555 = CIRCLE ( 'NONE', #12295, 4.999999999999997335 ) ;
#16556 = DIRECTION ( 'NONE',  ( 0.000000000000000000, 1.000000000000000000, 0.000000000000000000 ) ) ;
#16557 = CARTESIAN_POINT ( 'NONE',  ( -3.000000000000000888, 191.6227766016837961, 1.224646799147353454E-15 ) ) ;
#16558 =( GEOMETRIC_REPRESENTATION_CONTEXT ( 3 ) GLOBAL_UNCERTAINTY_ASSIGNED_CONTEXT ( ( #1007 ) ) GLOBAL_UNIT_ASSIGNED_CONTEXT ( ( #2734, #74, #17337 ) ) REPRESENTATION_CONTEXT ( 'NONE', 'WORKASPACE' ) );
#16559 = CARTESIAN_POINT ( 'NONE',  ( -78.47686795807116766, 201.3896308033655487, 14.24607874381215744 ) ) ;
#16560 = AXIS2_PLACEMENT_3D ( 'NONE', #13147, #6420, #10305 ) ;
#16561 = ORIENTED_EDGE ( 'NONE', *, *, #16038, .F. ) ;
#16562 = VERTEX_POINT ( 'NONE', #4950 ) ;
#16563 = DIRECTION ( 'NONE',  ( 0.000000000000000000, 1.000000000000000000, 0.000000000000000000 ) ) ;
#16564 = CARTESIAN_POINT ( 'NONE',  ( -27.99999999999998224, 10.00000000000000000, -28.00000000000000355 ) ) ;
#16565 = ORIENTED_EDGE ( 'NONE', *, *, #11491, .F. ) ;
#16566 = CARTESIAN_POINT ( 'NONE',  ( -24.93725393319379435, 120.0000000000000284, 5.500000000000000000 ) ) ;
#16567 = DIRECTION ( 'NONE',  ( 0.000000000000000000, 0.000000000000000000, -1.000000000000000000 ) ) ;
#16568 = VECTOR ( 'NONE', #2812, 1000.000000000000000 ) ;
#16569 = ORIENTED_EDGE ( 'NONE', *, *, #11007, .T. ) ;
#16570 = EDGE_CURVE ( 'NONE', #6571, #9979, #1230, .T. ) ;
#16571 = CIRCLE ( 'NONE', #5250, 12.00000000000000000 ) ;
#16572 = CARTESIAN_POINT ( 'NONE',  ( 37.05152766480231463, 199.2234891967518706, -18.10843944793624516 ) ) ;
#16573 = ADVANCED_FACE ( 'NONE', ( #17168 ), #13190, .F. ) ;
#16574 = CARTESIAN_POINT ( 'NONE',  ( -31.66708739526795924, 119.0000000000000284, 5.500000000000000000 ) ) ;
#16575 = DIRECTION ( 'NONE',  ( 0.000000000000000000, 0.000000000000000000, -1.000000000000000000 ) ) ;
#16576 = CARTESIAN_POINT ( 'NONE',  ( 49.99999999999998579, 167.6227766016838530, 8.071800142134975431 ) ) ;
#16577 = DIRECTION ( 'NONE',  ( 0.000000000000000000, 0.8660254037844413721, -0.4999999999999952816 ) ) ;
#16578 = CARTESIAN_POINT ( 'NONE',  ( -40.00000000000000000, 20.00000000000000000, 30.00000000000000355 ) ) ;
#16579 = EDGE_CURVE ( 'NONE', #15849, #12705, #16299, .T. ) ;
#16580 = CARTESIAN_POINT ( 'NONE',  ( -80.00000000000001421, 196.6227766016838245, 10.00000000000000178 ) ) ;
#16581 = TOROIDAL_SURFACE ( 'NONE', #8930, 740.0000000000000000, 10.00000000000000000 ) ;
#16582 = ORIENTED_EDGE ( 'NONE', *, *, #17290, .T. ) ;
#16583 = CARTESIAN_POINT ( 'NONE',  ( 17.91514137517177474, 140.8731888928338094, -16.72020691847105667 ) ) ;
#16584 = VECTOR ( 'NONE', #14214, 1000.000000000000000 ) ;
#16585 = ORIENTED_EDGE ( 'NONE', *, *, #3557, .F. ) ;
#16586 = CARTESIAN_POINT ( 'NONE',  ( -72.50000000000000000, 196.4352734575233228, -21.75827460206395614 ) ) ;
#16587 = CARTESIAN_POINT ( 'NONE',  ( -32.64269715136552463, 118.7804878048780779, -4.499999999999999112 ) ) ;
#16588 = ORIENTED_EDGE ( 'NONE', *, *, #11334, .F. ) ;
#16589 = ORIENTED_EDGE ( 'NONE', *, *, #12510, .T. ) ;
#16590 = LINE ( 'NONE', #2142, #6947 ) ;
#16591 = CARTESIAN_POINT ( 'NONE',  ( -38.00000000000000000, 20.00000000000000000, -28.00000000000000355 ) ) ;
#16592 = CYLINDRICAL_SURFACE ( 'NONE', #12941, 24.99999999999999645 ) ;
#16593 = VECTOR ( 'NONE', #6656, 1000.000000000000000 ) ;
#16594 = VECTOR ( 'NONE', #7014, 1000.000000000000000 ) ;
#16595 = ORIENTED_EDGE ( 'NONE', *, *, #13025, .T. ) ;
#16596 = DIRECTION ( 'NONE',  ( -0.000000000000000000, -0.000000000000000000, -1.000000000000000000 ) ) ;
#16597 = VECTOR ( 'NONE', #12293, 1000.000000000000000 ) ;
#16598 = MECHANICAL_DESIGN_GEOMETRIC_PRESENTATION_REPRESENTATION (  '', ( #1372 ), #3913 ) ;
#16599 = DIRECTION ( 'NONE',  ( -1.000000000000000000, 0.000000000000000000, 0.000000000000000000 ) ) ;
#16600 = AXIS2_PLACEMENT_3D ( 'NONE', #14510, #6361, #9105 ) ;
#16601 = CARTESIAN_POINT ( 'NONE',  ( -84.24272906227606939, 193.9598103731634353, 24.29383909379281192 ) ) ;
#16602 = DIRECTION ( 'NONE',  ( 1.000000000000000000, 0.000000000000000000, 0.000000000000000000 ) ) ;
#16603 = CARTESIAN_POINT ( 'NONE',  ( 15.97392895077415531, 29.97895215653467815, 12.94942366938410139 ) ) ;
#16604 = FACE_OUTER_BOUND ( 'NONE', #14665, .T. ) ;
#16605 = EDGE_CURVE ( 'NONE', #1820, #874, #13769, .T. ) ;
#16606 = EDGE_LOOP ( 'NONE', ( #14127, #7505, #9788, #7434, #2380 ) ) ;
#16607 = CARTESIAN_POINT ( 'NONE',  ( -75.92662808041686162, 201.0442424278814713, -18.96251499051319556 ) ) ;
#16608 = CARTESIAN_POINT ( 'NONE',  ( -90.33974596215564645, 171.6227766016838245, 0.000000000000000000 ) ) ;
#16609 = CARTESIAN_POINT ( 'NONE',  ( 32.29638371061065527, 20.00000000000000355, -15.01265034258821096 ) ) ;
#16610 = CARTESIAN_POINT ( 'NONE',  ( -153.0000000000000284, 171.6227766016838245, 0.000000000000000000 ) ) ;
#16611 = CARTESIAN_POINT ( 'NONE',  ( -95.00000000000000000, 171.6227766016838245, 0.000000000000000000 ) ) ;
#16612 = AXIS2_PLACEMENT_3D ( 'NONE', #10606, #13096, #13181 ) ;
#16613 = ORIENTED_EDGE ( 'NONE', *, *, #9265, .T. ) ;
#16614 = CIRCLE ( 'NONE', #8957, 2.499999999999998668 ) ;
#16615 = ORIENTED_EDGE ( 'NONE', *, *, #1993, .F. ) ;
#16616 = AXIS2_PLACEMENT_3D ( 'NONE', #7730, #15799, #1010 ) ;
#16617 = COLOUR_RGB ( '', 0.08235294, 0.09019608, 0.10196078) ;
#16618 = CARTESIAN_POINT ( 'NONE',  ( 6.134011831684059501, 144.1839557653415795, 18.33333333333333215 ) ) ;
#16619 = ADVANCED_FACE ( 'NONE', ( #4244 ), #9629, .F. ) ;
#16620 = ORIENTED_EDGE ( 'NONE', *, *, #9112, .F. ) ;
#16621 = DIRECTION ( 'NONE',  ( 1.000000000000000000, 0.000000000000000000, 0.000000000000000000 ) ) ;
#16622 = ADVANCED_FACE ( 'NONE', ( #1581 ), #14858, .F. ) ;
#16623 = VERTEX_POINT ( 'NONE', #5567 ) ;
#16624 = CARTESIAN_POINT ( 'NONE',  ( 21.99999999999998224, 9.999999999999998224, -30.00000000000001066 ) ) ;
#16625 = CARTESIAN_POINT ( 'NONE',  ( -725.0000000000000000, 30.00000000000000000, 25.00000000000000000 ) ) ;
#16626 = LINE ( 'NONE', #14843, #8999 ) ;
#16627 = B_SPLINE_CURVE_WITH_KNOTS ( 'NONE', 3,
 ( #3127, #8338, #376, #1530, #13755, #1717, #7025, #7110, #8525, #12245, #13932, #1795, #5869, #14902, #5521, #10909, #4198, #9585, #14989, #6929, #12333, #5612 ),
 .UNSPECIFIED., .F., .F.,
 ( 4, 2, 2, 2, 2, 2, 2, 2, 2, 2, 4 ),
 ( 0.000000000000000000, 0.001700754388868652408, 0.003401508777737304815, 0.005102263166605957440, 0.005952640361040282234, 0.006803017555474607028, 0.008503771944343253147, 0.01020452633321189927, 0.01190528072208054712, 0.01275565791651486931, 0.01360603511094918977 ),
 .UNSPECIFIED. ) ;
#16628 = DIRECTION ( 'NONE',  ( 0.000000000000000000, 0.000000000000000000, 1.000000000000000000 ) ) ;
#16629 = DIRECTION ( 'NONE',  ( 0.000000000000000000, 0.000000000000000000, 1.000000000000000000 ) ) ;
#16630 = VECTOR ( 'NONE', #13407, 1000.000000000000000 ) ;
#16631 = ORIENTED_EDGE ( 'NONE', *, *, #15468, .F. ) ;
#16632 = LINE ( 'NONE', #4499, #12938 ) ;
#16633 = DIRECTION ( 'NONE',  ( 0.000000000000000000, 0.000000000000000000, -1.000000000000000000 ) ) ;
#16634 = DIRECTION ( 'NONE',  ( -0.000000000000000000, -0.000000000000000000, 1.000000000000000000 ) ) ;
#16635 = LINE ( 'NONE', #13897, #13456 ) ;
#16636 = PRODUCT_DEFINITION_SHAPE ( 'NONE', 'NONE',  #17524 ) ;
#16637 = DIRECTION ( 'NONE',  ( -1.000000000000000000, 0.000000000000000000, 0.000000000000000000 ) ) ;
#16638 = EDGE_CURVE ( 'NONE', #1130, #16300, #10651, .T. ) ;
#16639 = ADVANCED_FACE ( 'NONE', ( #9540, #8391, #9714, #14945, #12288, #15111, #2907, #5401, #5742, #6980, #7074, #2993, #255, #13540 ), #5657, .F. ) ;
#16640 = CIRCLE ( 'NONE', #2782, 5.000000000000000888 ) ;
#16641 = ADVANCED_FACE ( 'NONE', ( #3085 ), #9810, .T. ) ;
#16642 = ORIENTED_EDGE ( 'NONE', *, *, #12573, .F. ) ;
#16643 = DIRECTION ( 'NONE',  ( 1.000000000000000000, 0.000000000000000000, 0.000000000000000000 ) ) ;
#16644 = CIRCLE ( 'NONE', #8145, 4.750000000000000000 ) ;
#16645 = PRESENTATION_LAYER_ASSIGNMENT (  '', '', ( #13811 ) ) ;
#16646 = ORIENTED_EDGE ( 'NONE', *, *, #15921, .F. ) ;
#16647 = CARTESIAN_POINT ( 'NONE',  ( 21.93446201513734550, 139.6105936900751203, 14.17700481206107455 ) ) ;
#16648 = CARTESIAN_POINT ( 'NONE',  ( 48.00000000000000711, 175.6227766016838245, 8.071800142134975431 ) ) ;
#16649 = CARTESIAN_POINT ( 'NONE',  ( -208.1430079281944074, 176.3671987152221448, -3.647967993167786194 ) ) ;
#16650 = DIRECTION ( 'NONE',  ( 0.000000000000000000, 0.000000000000000000, 1.000000000000000000 ) ) ;
#16651 = CARTESIAN_POINT ( 'NONE',  ( -15.00000000000002132, 90.00000000000000000, 4.999999999999999112 ) ) ;
#16652 = CARTESIAN_POINT ( 'NONE',  ( 20.96141083122825322, 29.88026331201747254, 10.28670731940101923 ) ) ;
#16653 = CIRCLE ( 'NONE', #15501, 2.500000000000000444 ) ;
#16654 = CARTESIAN_POINT ( 'NONE',  ( -74.99999999999998579, 197.2379877313572081, 20.82664773619437071 ) ) ;
#16655 = AXIS2_PLACEMENT_3D ( 'NONE', #5646, #16271, #4141 ) ;
#16656 = SURFACE_STYLE_FILL_AREA ( #11063 ) ;
#16657 = ORIENTED_EDGE ( 'NONE', *, *, #6923, .T. ) ;
#16658 = ORIENTED_EDGE ( 'NONE', *, *, #3571, .T. ) ;
#16659 = CARTESIAN_POINT ( 'NONE',  ( 25.06493225413665016, 20.00000000000000000, -5.000000000000004441 ) ) ;
#16660 = CARTESIAN_POINT ( 'NONE',  ( 26.01985846803728464, 139.8002605074728990, -8.764508151440994155 ) ) ;
#16661 = ORIENTED_EDGE ( 'NONE', *, *, #9137, .T. ) ;
#16662 = CARTESIAN_POINT ( 'NONE',  ( -26.90043998676167192, 19.99999999999999645, 11.53672424425260878 ) ) ;
#16663 = DIRECTION ( 'NONE',  ( -1.000000000000000000, -0.000000000000000000, -0.000000000000000000 ) ) ;
#16664 = AXIS2_PLACEMENT_3D ( 'NONE', #7424, #10251, #12826 ) ;
#16665 = ORIENTED_EDGE ( 'NONE', *, *, #7160, .F. ) ;
#16666 = AXIS2_PLACEMENT_3D ( 'NONE', #2801, #1554, #17504 ) ;
#16667 = CARTESIAN_POINT ( 'NONE',  ( 27.73879888791969961, 153.7971187266995230, -27.77174765869275319 ) ) ;
#16668 = CIRCLE ( 'NONE', #12978, 2.499999999999998668 ) ;
#16669 = CARTESIAN_POINT ( 'NONE',  ( -27.98221281347037959, 18.00000000000000711, 5.670874406215274277 ) ) ;
#16670 = CARTESIAN_POINT ( 'NONE',  ( -208.1243153690002714, 166.1146168224391886, -2.051539466268182732 ) ) ;
#16671 = LINE ( 'NONE', #9838, #2122 ) ;
#16672 = CARTESIAN_POINT ( 'NONE',  ( -68.00000000000000000, 154.3022685259950038, -9.999999999999900524 ) ) ;
#16673 = CARTESIAN_POINT ( 'NONE',  ( 1.559999999999998943, -0.8660254037844428154, -1.499999999999997780 ) ) ;
#16674 = DIRECTION ( 'NONE',  ( -0.000000000000000000, -0.000000000000000000, -1.000000000000000000 ) ) ;
#16675 = VERTEX_POINT ( 'NONE', #10960 ) ;
#16676 = DIRECTION ( 'NONE',  ( 1.000000000000000000, -0.000000000000000000, -0.000000000000000000 ) ) ;
#16677 = VECTOR ( 'NONE', #4760, 1000.000000000000000 ) ;
#16678 = VECTOR ( 'NONE', #6835, 1000.000000000000000 ) ;
#16679 = ORIENTED_EDGE ( 'NONE', *, *, #302, .T. ) ;
#16680 = EDGE_CURVE ( 'NONE', #4370, #15922, #1896, .T. ) ;
#16681 = CARTESIAN_POINT ( 'NONE',  ( -5.000000000000000888, 154.3022685259950038, 9.999999999999900524 ) ) ;
#16682 = FACE_OUTER_BOUND ( 'NONE', #9024, .T. ) ;
#16683 = ORIENTED_EDGE ( 'NONE', *, *, #13974, .T. ) ;
#16684 = DIRECTION ( 'NONE',  ( 0.000000000000000000, -1.000000000000000000, 0.000000000000000000 ) ) ;
#16685 = CARTESIAN_POINT ( 'NONE',  ( 1.559999999999998943, -0.8660254037844428154, 1.500000000000001332 ) ) ;
#16686 = CARTESIAN_POINT ( 'NONE',  ( 14.69130379018311316, 137.7259585328908713, 10.44822943247861602 ) ) ;
#16687 = CIRCLE ( 'NONE', #10454, 5.000000000000000888 ) ;
#16688 = ORIENTED_EDGE ( 'NONE', *, *, #3062, .T. ) ;
#16689 = DIRECTION ( 'NONE',  ( -1.000000000000000000, 0.000000000000000000, 0.000000000000000000 ) ) ;
#16690 = AXIS2_PLACEMENT_3D ( 'NONE', #6342, #17415, #9089 ) ;
#16691 = DIRECTION ( 'NONE',  ( -0.000000000000000000, -0.000000000000000000, -1.000000000000000000 ) ) ;
#16692 = DIRECTION ( 'NONE',  ( 1.000000000000000000, 0.000000000000000000, 0.000000000000000000 ) ) ;
#16693 = CARTESIAN_POINT ( 'NONE',  ( 49.99999999999998579, 179.6227766016838245, 12.50000337241049309 ) ) ;
#16694 = CARTESIAN_POINT ( 'NONE',  ( 16.61976933981454962, 29.96600215813370838, 12.82127072618890118 ) ) ;
#16695 = CARTESIAN_POINT ( 'NONE',  ( -7.379000772444995526, 18.00000000000000355, -12.99999999999999822 ) ) ;
#16696 = ORIENTED_EDGE ( 'NONE', *, *, #9111, .F. ) ;
#16697 = CARTESIAN_POINT ( 'NONE',  ( 27.44407568426044008, 138.8271129316868837, -3.666666666666658081 ) ) ;
#16698 = CARTESIAN_POINT ( 'NONE',  ( -48.00000000000000000, 206.6227766016838245, 2.143131898507868248E-15 ) ) ;
#16699 = VERTEX_POINT ( 'NONE', #15209 ) ;
#16700 = EDGE_CURVE ( 'NONE', #8437, #12225, #2745, .T. ) ;
#16701 = FACE_OUTER_BOUND ( 'NONE', #15692, .T. ) ;
#16702 = PLANE ( 'NONE',  #15438 ) ;
#16703 = AXIS2_PLACEMENT_3D ( 'NONE', #9692, #14928, #16356 ) ;
#16704 = AXIS2_PLACEMENT_3D ( 'NONE', #10310, #941, #5011 ) ;
#16705 = ORIENTED_EDGE ( 'NONE', *, *, #4333, .T. ) ;
#16706 = EDGE_LOOP ( 'NONE', ( #14376, #13712, #15884, #13491 ) ) ;
#16707 = CIRCLE ( 'NONE', #4833, 1.000000000000000888 ) ;
#16708 = EDGE_CURVE ( 'NONE', #10629, #6881, #1028, .T. ) ;
#16709 = CARTESIAN_POINT ( 'NONE',  ( 0.000000000000000000, 18.00000000000000355, 0.000000000000000000 ) ) ;
#16710 = ORIENTED_EDGE ( 'NONE', *, *, #15377, .T. ) ;
#16711 = EDGE_CURVE ( 'NONE', #6145, #11303, #7539, .T. ) ;
#16712 = DIRECTION ( 'NONE',  ( 0.000000000000000000, 0.000000000000000000, -1.000000000000000000 ) ) ;
#16713 = EDGE_CURVE ( 'NONE', #14743, #9236, #12741, .T. ) ;
#16714 = ORIENTED_EDGE ( 'NONE', *, *, #8565, .T. ) ;
#16715 = CARTESIAN_POINT ( 'NONE',  ( -38.00000000000000000, 20.00000000000000000, 0.000000000000000000 ) ) ;
#16716 = CYLINDRICAL_SURFACE ( 'NONE', #3265, 12.00000000000000000 ) ;
#16717 = DIRECTION ( 'NONE',  ( 0.000000000000000000, 0.000000000000000000, 1.000000000000000000 ) ) ;
#16718 = VECTOR ( 'NONE', #1996, 1000.000000000000000 ) ;
#16719 = CARTESIAN_POINT ( 'NONE',  ( 35.59781103574917438, 141.6107120069883365, -13.74530841833676931 ) ) ;
#16720 = VERTEX_POINT ( 'NONE', #517 ) ;
#16721 = CARTESIAN_POINT ( 'NONE',  ( 27.76496263192228042, 142.1468147500166594, 14.83914868552980160 ) ) ;
#16722 = DIRECTION ( 'NONE',  ( -1.000000000000000000, -0.000000000000000000, -0.000000000000000000 ) ) ;
#16723 = DIRECTION ( 'NONE',  ( 0.000000000000000000, 0.000000000000000000, -1.000000000000000000 ) ) ;
#16724 = CARTESIAN_POINT ( 'NONE',  ( -16.41264213764281976, 19.99999999999999645, -23.02790928165778794 ) ) ;
#16725 =( NAMED_UNIT ( * ) PLANE_ANGLE_UNIT ( ) SI_UNIT ( $, .RADIAN. ) );
#16726 = AXIS2_PLACEMENT_3D ( 'NONE', #16439, #5532, #10923 ) ;
#16727 = DIRECTION ( 'NONE',  ( -0.08715574274764661955, -0.4980973490458647235, -0.8627299156628267518 ) ) ;
#16728 = VERTEX_POINT ( 'NONE', #12907 ) ;
#16729 = CARTESIAN_POINT ( 'NONE',  ( 39.99999999999998579, -20.00000000000000000, -35.00000000000002132 ) ) ;
#16730 = VERTEX_POINT ( 'NONE', #16984 ) ;
#16731 = CARTESIAN_POINT ( 'NONE',  ( -16.30611068361787019, 32.76923076923078781, 15.00000000000000000 ) ) ;
#16732 = ORIENTED_EDGE ( 'NONE', *, *, #12549, .T. ) ;
#16733 = CARTESIAN_POINT ( 'NONE',  ( -95.00000000000000000, 199.3133755249253056, -1.695560166891042033E-15 ) ) ;
#16734 = CARTESIAN_POINT ( 'NONE',  ( -50.00000000000000000, 171.6227766016838245, -2.296212748401287183E-15 ) ) ;
#16735 = ORIENTED_EDGE ( 'NONE', *, *, #13863, .F. ) ;
#16736 = LINE ( 'NONE', #15482, #17166 ) ;
#16737 = VECTOR ( 'NONE', #3202, 1000.000000000000000 ) ;
#16738 = DIRECTION ( 'NONE',  ( 1.000000000000000000, -0.000000000000000000, -0.000000000000000000 ) ) ;
#16739 = EDGE_CURVE ( 'NONE', #7107, #919, #15378, .T. ) ;
#16740 = EDGE_CURVE ( 'NONE', #8740, #374, #4999, .T. ) ;
#16741 = FACE_OUTER_BOUND ( 'NONE', #5774, .T. ) ;
#16742 = EDGE_CURVE ( 'NONE', #1481, #1803, #2096, .T. ) ;
#16743 = FACE_BOUND ( 'NONE', #11753, .T. ) ;
#16744 = ORIENTED_EDGE ( 'NONE', *, *, #10406, .T. ) ;
#16745 = ORIENTED_EDGE ( 'NONE', *, *, #1918, .F. ) ;
#16746 = CYLINDRICAL_SURFACE ( 'NONE', #10895, 5.000000000000000888 ) ;
#16747 = CARTESIAN_POINT ( 'NONE',  ( 22.64347415271929265, 141.1870565414818941, -12.76399958404563684 ) ) ;
#16748 = ORIENTED_EDGE ( 'NONE', *, *, #7458, .F. ) ;
#16749 = CARTESIAN_POINT ( 'NONE',  ( 2.950000000000001066, 0.000000000000000000, 0.000000000000000000 ) ) ;
#16750 = CARTESIAN_POINT ( 'NONE',  ( 33.99999999999998579, 9.999999999999998224, -30.00000000000001066 ) ) ;
#16751 = ORIENTED_EDGE ( 'NONE', *, *, #5854, .F. ) ;
#16752 = DIRECTION ( 'NONE',  ( 0.000000000000000000, 0.000000000000000000, 1.000000000000000000 ) ) ;
#16753 = CARTESIAN_POINT ( 'NONE',  ( 48.00000000000000000, 196.6227766016838245, 0.000000000000000000 ) ) ;
#16754 = CARTESIAN_POINT ( 'NONE',  ( 49.99999999999998579, 159.6227766016838814, -5.571800142134975431 ) ) ;
#16755 = DIRECTION ( 'NONE',  ( -1.000000000000000000, 0.000000000000000000, 0.000000000000000000 ) ) ;
#16756 = CARTESIAN_POINT ( 'NONE',  ( -90.80384757729339640, 204.6227766016838245, 0.000000000000000000 ) ) ;
#16757 = EDGE_CURVE ( 'NONE', #13060, #2291, #2446, .T. ) ;
#16758 = EDGE_CURVE ( 'NONE', #1219, #9311, #8660, .T. ) ;
#16759 = CARTESIAN_POINT ( 'NONE',  ( 14.93242934743710393, 30.00000000000000000, -25.00000000000000000 ) ) ;
#16760 = ADVANCED_FACE ( 'NONE', ( #11315 ), #6977, .F. ) ;
#16761 = CARTESIAN_POINT ( 'NONE',  ( -80.00000000000001421, 196.6227766016838245, -16.00000000000000000 ) ) ;
#16762 = ORIENTED_EDGE ( 'NONE', *, *, #13334, .F. ) ;
#16763 = CARTESIAN_POINT ( 'NONE',  ( -45.00000000000000711, 171.6227766016838245, 0.000000000000000000 ) ) ;
#16764 = ORIENTED_EDGE ( 'NONE', *, *, #17060, .T. ) ;
#16765 = CARTESIAN_POINT ( 'NONE',  ( 39.99999999999998579, 4.000000000000000000, -30.00000000000000000 ) ) ;
#16766 = CARTESIAN_POINT ( 'NONE',  ( 27.75000000000000000, 2.789133085058096608E-16, -2.055000000000000160 ) ) ;
#16767 = ORIENTED_EDGE ( 'NONE', *, *, #14847, .F. ) ;
#16768 = CARTESIAN_POINT ( 'NONE',  ( 34.42405209918207731, 19.99999999999999289, 9.535225002503356251 ) ) ;
#16769 = CARTESIAN_POINT ( 'NONE',  ( -74.10786375645523094, 201.2861607625692102, -14.48320912595414889 ) ) ;
#16770 = CARTESIAN_POINT ( 'NONE',  ( 15.93460003626540100, 136.8193095811535045, 3.708327557688629650 ) ) ;
#16771 = ORIENTED_EDGE ( 'NONE', *, *, #4335, .T. ) ;
#16772 = CONTEXT_DEPENDENT_SHAPE_REPRESENTATION ( #10937, #15349 ) ;
#16773 = DIRECTION ( 'NONE',  ( -1.000000000000000000, -3.469446951953614189E-16, 0.000000000000000000 ) ) ;
#16774 = ADVANCED_FACE ( 'NONE', ( #783 ), #8831, .F. ) ;
#16775 = CYLINDRICAL_SURFACE ( 'NONE', #9784, 20.00000000000000355 ) ;
#16776 = CARTESIAN_POINT ( 'NONE',  ( -75.34838324441767554, 194.7673412502506096, 23.52603474534219430 ) ) ;
#16777 = CARTESIAN_POINT ( 'NONE',  ( 48.00000000000000711, 175.6227766016838245, -3.071800142134975431 ) ) ;
#16778 = DIRECTION ( 'NONE',  ( 0.000000000000000000, 0.000000000000000000, 1.000000000000000000 ) ) ;
#16779 = FACE_OUTER_BOUND ( 'NONE', #12645, .T. ) ;
#16780 = ORIENTED_EDGE ( 'NONE', *, *, #6112, .F. ) ;
#16781 = DIRECTION ( 'NONE',  ( -1.000000000000000000, -0.000000000000000000, -0.000000000000000000 ) ) ;
#16782 = DIRECTION ( 'NONE',  ( 0.000000000000000000, 0.000000000000000000, -1.000000000000000000 ) ) ;
#16783 = ORIENTED_EDGE ( 'NONE', *, *, #1862, .T. ) ;
#16784 = LINE ( 'NONE', #4649, #5348 ) ;
#16785 = DIRECTION ( 'NONE',  ( 0.000000000000000000, 0.000000000000000000, 1.000000000000000000 ) ) ;
#16786 = ORIENTED_EDGE ( 'NONE', *, *, #7458, .T. ) ;
#16787 = ORIENTED_EDGE ( 'NONE', *, *, #14223, .F. ) ;
#16788 = VERTEX_POINT ( 'NONE', #420 ) ;
#16789 = CARTESIAN_POINT ( 'NONE',  ( 7.863372401969320968, 140.4786490112420552, 12.74411896114139076 ) ) ;
#16790 = EDGE_LOOP ( 'NONE', ( #6456, #14265, #3541, #14048 ) ) ;
#16791 = ORIENTED_EDGE ( 'NONE', *, *, #4924, .T. ) ;
#16792 = CARTESIAN_POINT ( 'NONE',  ( -3.000000000000000888, 171.6227766016838245, 0.000000000000000000 ) ) ;
#16793 = EDGE_CURVE ( 'NONE', #10702, #17386, #2166, .T. ) ;
#16794 = DIRECTION ( 'NONE',  ( -1.000000000000000000, -0.000000000000000000, -0.000000000000000000 ) ) ;
#16795 = DIRECTION ( 'NONE',  ( 1.000000000000000000, 0.000000000000000000, 0.000000000000000000 ) ) ;
#16796 = CARTESIAN_POINT ( 'NONE',  ( 39.99999999999998579, 8.000000000000007105, 30.00000000000001066 ) ) ;
#16797 = VERTEX_POINT ( 'NONE', #6007 ) ;
#16798 = CARTESIAN_POINT ( 'NONE',  ( 33.42618164656464330, 142.9679699711796275, 16.37278862731308493 ) ) ;
#16799 = FACE_OUTER_BOUND ( 'NONE', #14293, .T. ) ;
#16800 = FACE_BOUND ( 'NONE', #10735, .T. ) ;
#16801 = EDGE_CURVE ( 'NONE', #1199, #13709, #611, .T. ) ;
#16802 = DIRECTION ( 'NONE',  ( 1.000000000000000000, 0.000000000000000000, 0.000000000000000000 ) ) ;
#16803 = DIRECTION ( 'NONE',  ( -1.156482317317868274E-16, 1.000000000000000000, 0.000000000000000000 ) ) ;
#16804 = EDGE_CURVE ( 'NONE', #4853, #1445, #8905, .T. ) ;
#16805 = DIRECTION ( 'NONE',  ( -0.000000000000000000, -0.000000000000000000, 1.000000000000000000 ) ) ;
#16806 = VERTEX_POINT ( 'NONE', #10158 ) ;
#16807 = CARTESIAN_POINT ( 'NONE',  ( -38.00000000000000000, 18.00000000000000355, -28.00000000000000355 ) ) ;
#16808 = AXIS2_PLACEMENT_3D ( 'NONE', #748, #5884, #5978 ) ;
#16809 = ORIENTED_EDGE ( 'NONE', *, *, #14822, .F. ) ;
#16810 = DIRECTION ( 'NONE',  ( -1.156482317317868274E-16, 1.000000000000000000, 0.000000000000000000 ) ) ;
#16811 = CIRCLE ( 'NONE', #7742, 2.499999999999998668 ) ;
#16812 = DIRECTION ( 'NONE',  ( 1.000000000000000000, 0.000000000000000000, 0.000000000000000000 ) ) ;
#16813 = CARTESIAN_POINT ( 'NONE',  ( -45.00000000000000000, 140.0000000000000000, 15.00000000000000000 ) ) ;
#16814 = EDGE_LOOP ( 'NONE', ( #8040, #15788 ) ) ;
#16815 = FACE_BOUND ( 'NONE', #6540, .T. ) ;
#16816 = CARTESIAN_POINT ( 'NONE',  ( 0.000000000000000000, 2.375000000000000000, 0.000000000000000000 ) ) ;
#16817 = CARTESIAN_POINT ( 'NONE',  ( -24.94987437106622252, 120.0000000000000284, -6.000000000000001776 ) ) ;
#16818 = CARTESIAN_POINT ( 'NONE',  ( 25.00907797400832777, 199.9711820797445512, -20.53336423377503195 ) ) ;
#16819 = AXIS2_PLACEMENT_3D ( 'NONE', #2485, #6288, #7529 ) ;
#16820 = VERTEX_POINT ( 'NONE', #16807 ) ;
#16821 = AXIS2_PLACEMENT_3D ( 'NONE', #12586, #2939, #12418 ) ;
#16822 = ORIENTED_EDGE ( 'NONE', *, *, #14003, .T. ) ;
#16823 = CARTESIAN_POINT ( 'NONE',  ( 21.36708699129162881, 19.99999999999999645, -23.94811280430947420 ) ) ;
#16824 = CARTESIAN_POINT ( 'NONE',  ( 27.32038637416026816, 139.0270950805171424, -5.204462201318943215 ) ) ;
#16825 = EDGE_LOOP ( 'NONE', ( #9782, #9412, #11732, #6126 ) ) ;
#16826 = FACE_OUTER_BOUND ( 'NONE', #2519, .T. ) ;
#16827 = CARTESIAN_POINT ( 'NONE',  ( 8.147273376221958685, 133.4207317082267537, -12.78321197947435728 ) ) ;
#16828 = ORIENTED_EDGE ( 'NONE', *, *, #5535, .T. ) ;
#16829 = EDGE_CURVE ( 'NONE', #9334, #3758, #13121, .T. ) ;
#16830 = CARTESIAN_POINT ( 'NONE',  ( 32.50000000000000711, 146.6227766016838245, 0.000000000000000000 ) ) ;
#16831 = AXIS2_PLACEMENT_3D ( 'NONE', #813, #15590, #10351 ) ;
#16832 = AXIS2_PLACEMENT_3D ( 'NONE', #5939, #15126, #9727 ) ;
#16833 = DIRECTION ( 'NONE',  ( 1.000000000000000000, 0.000000000000000000, 0.000000000000000000 ) ) ;
#16834 = CARTESIAN_POINT ( 'NONE',  ( -43.00000000000000000, 130.0000000000000000, 0.000000000000000000 ) ) ;
#16835 = CARTESIAN_POINT ( 'NONE',  ( -11.94789857657465681, 17.99999999999885603, 9.192893430571174918 ) ) ;
#16836 = DIRECTION ( 'NONE',  ( 1.000000000000000000, 0.000000000000000000, 0.000000000000000000 ) ) ;
#16837 = CARTESIAN_POINT ( 'NONE',  ( 225.0000000000000000, 89.99999999999997158, 0.000000000000000000 ) ) ;
#16838 = ORIENTED_EDGE ( 'NONE', *, *, #3285, .T. ) ;
#16839 = DIRECTION ( 'NONE',  ( -0.000000000000000000, -0.000000000000000000, -1.000000000000000000 ) ) ;
#16840 = ORIENTED_EDGE ( 'NONE', *, *, #8773, .F. ) ;
#16841 = DIRECTION ( 'NONE',  ( -1.000000000000000000, -0.000000000000000000, -0.000000000000000000 ) ) ;
#16842 = COLOUR_RGB ( '', 0.31764706, 0.68627451, 0.89019608) ;
#16843 = FACE_BOUND ( 'NONE', #15157, .T. ) ;
#16844 = AXIS2_PLACEMENT_3D ( 'NONE', #8993, #15635, #10152 ) ;
#16845 = EDGE_LOOP ( 'NONE', ( #4712, #11871, #13566, #12396, #2252, #9406, #9242, #2766, #2698, #14881, #1818, #17164, #14267, #4804 ) ) ;
#16846 = CARTESIAN_POINT ( 'NONE',  ( -100.0000000000000000, 134.2062027339443944, -25.00000000000000000 ) ) ;
#16847 = AXIS2_PLACEMENT_3D ( 'NONE', #3130, #16090, #15339 ) ;
#16848 = EDGE_CURVE ( 'NONE', #1445, #583, #13204, .T. ) ;
#16849 = ADVANCED_FACE ( 'NONE', ( #11221 ), #14236, .T. ) ;
#16850 = CARTESIAN_POINT ( 'NONE',  ( 20.21654089865888437, 29.92961455958988637, 13.49713695059922891 ) ) ;
#16851 = ADVANCED_FACE ( 'NONE', ( #3177 ), #13977, .T. ) ;
#16852 = CARTESIAN_POINT ( 'NONE',  ( 196.0000000000000000, 175.6227766016838530, -16.92820660268601429 ) ) ;
#16853 = ORIENTED_EDGE ( 'NONE', *, *, #8803, .F. ) ;
#16854 = PLANE ( 'NONE',  #13031 ) ;
#16855 = CYLINDRICAL_SURFACE ( 'NONE', #5822, 2.500000000000002220 ) ;
#16856 = CLOSED_SHELL ( 'NONE', ( #11796, #5680, #14850, #2023, #6557, #16920, #1053, #933, #4994, #4656, #10132, #9907, #5575, #8351, #3212, #219, #13653, #11803, #5988, #5668, #2330, #15640, #14040, #3755, #6953, #16641, #15226, #5670, #1743, #8387, #11006, #1032, #16000, #3380, #11104, #16484, #9970, #12991, #2677, #2128, #8550, #6235, #4622, #6343, #15932, #15525, #9786, #6889, #3053, #10882, #9139, #10668, #14166, #4746, #5272, #14560, #8462, #7812, #13983, #11967, #15068, #173, #11312, #125, #7017, #11984, #8917, #2898, #1195, #7664, #1764, #13459, #2182, #12492, #16142, #17450, #721, #14164, #5993, #14540, #15607, #3920, #6203, #1777, #6050, #10148, #11367, #2273, #14735, #9806, #1315, #11166, #4674, #3261, #13233, #470, #1673, #8776, #16921, #4782, #9679, #2656, #9962, #1575, #392, #13113, #7153, #5155, #1253, #9549, #3533, #8682, #14909, #17463, #3252, #11420, #3860, #16957, #13388, #14303, #779, #7523, #4873, #14346, #4031, #3168, #2496, #13920, #7269, #3697, #14852, #6016, #14387, #17106, #7917, #12933, #8029, #15986, #1768, #10442, #4790, #6474, #13169, #11110, #8804, #7717, #4602, #11862, #15612, #2385, #9774, #12282, #16448, #7491, #10243, #15225, #11275, #16533, #8228, #4948, #15552, #10560, #15611, #16426, #14078, #3213, #8226, #14629, #7177, #4039, #7279, #3474, #16916, #8814, #9405, #17161, #2350, #4998, #2456, #10955, #865, #2300, #3458, #5656, #1817, #16234, #910 ) ) ;
#16857 = AXIS2_PLACEMENT_3D ( 'NONE', #914, #6390, #5161 ) ;
#16858 = CARTESIAN_POINT ( 'NONE',  ( -82.06570270424580826, 192.0656250386302020, 25.90562197801994060 ) ) ;
#16859 = CARTESIAN_POINT ( 'NONE',  ( -18.25212770525996930, 32.30769230769229949, -5.349717987761776428 ) ) ;
#16860 = CARTESIAN_POINT ( 'NONE',  ( -20.00000000000000355, 171.6227766016838245, 0.000000000000000000 ) ) ;
#16861 = AXIS2_PLACEMENT_3D ( 'NONE', #7215, #9513, #8970 ) ;
#16862 = DIRECTION ( 'NONE',  ( -1.000000000000000000, -0.000000000000000000, -0.000000000000000000 ) ) ;
#16863 = ORIENTED_EDGE ( 'NONE', *, *, #7151, .T. ) ;
#16864 = CARTESIAN_POINT ( 'NONE',  ( -32.66708739526796990, 100.9060348297503538, 4.814896201975309431 ) ) ;
#16865 = CARTESIAN_POINT ( 'NONE',  ( 27.99999999999998224, 9.999999999999998224, 0.000000000000000000 ) ) ;
#16866 = ORIENTED_EDGE ( 'NONE', *, *, #14180, .T. ) ;
#16867 = CARTESIAN_POINT ( 'NONE',  ( -91.33974596215563224, 136.6227766016838245, 0.000000000000000000 ) ) ;
#16868 = FACE_OUTER_BOUND ( 'NONE', #9157, .T. ) ;
#16869 = VERTEX_POINT ( 'NONE', #1841 ) ;
#16870 = ORIENTED_EDGE ( 'NONE', *, *, #3798, .T. ) ;
#16871 = AXIS2_PLACEMENT_3D ( 'NONE', #4874, #897, #10529 ) ;
#16872 = AXIS2_PLACEMENT_3D ( 'NONE', #3727, #5409, #14608 ) ;
#16873 = EDGE_LOOP ( 'NONE', ( #14043, #15481 ) ) ;
#16874 =( NAMED_UNIT ( * ) PLANE_ANGLE_UNIT ( ) SI_UNIT ( $, .RADIAN. ) );
#16875 = AXIS2_PLACEMENT_3D ( 'NONE', #8847, #12759, #8928 ) ;
#16876 = VERTEX_POINT ( 'NONE', #14158 ) ;
#16877 = PRESENTATION_STYLE_ASSIGNMENT (( #7477 ) ) ;
#16878 = FACE_OUTER_BOUND ( 'NONE', #15208, .T. ) ;
#16879 = CARTESIAN_POINT ( 'NONE',  ( 9.186438336152177087, 132.7758989760081931, 12.51111164240594675 ) ) ;
#16880 = DIRECTION ( 'NONE',  ( 1.000000000000000000, -0.000000000000000000, -0.000000000000000000 ) ) ;
#16881 = CARTESIAN_POINT ( 'NONE',  ( 30.49999999999998224, 9.999999999999998224, 0.000000000000000000 ) ) ;
#16882 = ORIENTED_EDGE ( 'NONE', *, *, #9111, .T. ) ;
#16883 = CARTESIAN_POINT ( 'NONE',  ( 25.40874610515435705, 144.6221806392915141, 18.97834816100454702 ) ) ;
#16884 = DIRECTION ( 'NONE',  ( 0.000000000000000000, 0.000000000000000000, 1.000000000000000000 ) ) ;
#16885 = AXIS2_PLACEMENT_3D ( 'NONE', #8230, #16295, #4167 ) ;
#16886 = DIRECTION ( 'NONE',  ( 0.000000000000000000, 0.000000000000000000, 1.000000000000000000 ) ) ;
#16887 = AXIS2_PLACEMENT_3D ( 'NONE', #9243, #11637, #13235 ) ;
#16888 = LINE ( 'NONE', #4764, #11730 ) ;
#16889 = EDGE_CURVE ( 'NONE', #11331, #3796, #7417, .T. ) ;
#16890 = EDGE_CURVE ( 'NONE', #17452, #10732, #15886, .T. ) ;
#16891 = DIRECTION ( 'NONE',  ( 0.000000000000000000, 0.000000000000000000, -1.000000000000000000 ) ) ;
#16892 = ORIENTED_EDGE ( 'NONE', *, *, #2107, .T. ) ;
#16893 = CARTESIAN_POINT ( 'NONE',  ( -95.00000000000000000, 143.9321776784423150, -5.086680500673126297E-15 ) ) ;
#16894 = VERTEX_POINT ( 'NONE', #17056 ) ;
#16895 = AXIS2_PLACEMENT_3D ( 'NONE', #7833, #14305, #1115 ) ;
#16896 = CARTESIAN_POINT ( 'NONE',  ( 11.02544963116560517, 142.2295695439714791, 19.00161275228506952 ) ) ;
#16897 = AXIS2_PLACEMENT_3D ( 'NONE', #9623, #12467, #15201 ) ;
#16898 = EDGE_CURVE ( 'NONE', #9236, #8681, #2549, .T. ) ;
#16899 = DIRECTION ( 'NONE',  ( 1.000000000000000000, 0.000000000000000000, 0.000000000000000000 ) ) ;
#16900 = MANIFOLD_SOLID_BREP ( 'Fillet1', #9783 ) ;
#16901 = CARTESIAN_POINT ( 'NONE',  ( 6.471945315774715546, 134.1315750335306518, -12.99999999999999822 ) ) ;
#16902 = ORIENTED_EDGE ( 'NONE', *, *, #6233, .T. ) ;
#16903 = CARTESIAN_POINT ( 'NONE',  ( 40.00000000000000711, 0.000000000000000000, 0.000000000000000000 ) ) ;
#16904 = CYLINDRICAL_SURFACE ( 'NONE', #6768, 19.49999999999998934 ) ;
#16905 = CARTESIAN_POINT ( 'NONE',  ( -79.54766608249138926, 201.6036812327912457, 13.78933345224466933 ) ) ;
#16906 = EDGE_LOOP ( 'NONE', ( #4832, #12435, #3429, #5851, #5522, #1882, #362 ) ) ;
#16907 = VECTOR ( 'NONE', #10474, 1000.000000000000000 ) ;
#16908 = ORIENTED_EDGE ( 'NONE', *, *, #3325, .T. ) ;
#16909 = EDGE_CURVE ( 'NONE', #11936, #14757, #12008, .T. ) ;
#16910 = CARTESIAN_POINT ( 'NONE',  ( 20.21654089865888437, 29.92961455958988637, -13.49713695059922891 ) ) ;
#16911 = CIRCLE ( 'NONE', #14366, 2.499999999999998668 ) ;
#16912 = DIRECTION ( 'NONE',  ( -1.000000000000000000, -0.000000000000000000, -0.000000000000000000 ) ) ;
#16913 = EDGE_LOOP ( 'NONE', ( #2961, #11980, #3457, #4836 ) ) ;
#16914 = CARTESIAN_POINT ( 'NONE',  ( -73.00000000000001421, 171.6227766016838245, 0.000000000000000000 ) ) ;
#16915 = CARTESIAN_POINT ( 'NONE',  ( 196.0000000000000000, 167.6227766016838530, 3.071800142134975431 ) ) ;
#16916 = ADVANCED_FACE ( 'NONE', ( #13348, #5192 ), #2359, .F. ) ;
#16917 = EDGE_LOOP ( 'NONE', ( #9015, #14827, #12921, #9261 ) ) ;
#16918 = CARTESIAN_POINT ( 'NONE',  ( 27.99999999999998224, 9.999999999999998224, -16.00000000000000000 ) ) ;
#16919 = UNCERTAINTY_MEASURE_WITH_UNIT (LENGTH_MEASURE( 1.000000000000000082E-05 ), #12805, 'distance_accuracy_value', 'NONE');
#16920 = ADVANCED_FACE ( 'NONE', ( #3608 ), #3698, .F. ) ;
#16921 = ADVANCED_FACE ( 'NONE', ( #7585, #15907, #10584 ), #14411, .T. ) ;
#16922 = AXIS2_PLACEMENT_3D ( 'NONE', #1623, #16497, #9751 ) ;
#16923 = AXIS2_PLACEMENT_3D ( 'NONE', #525, #16812, #4774 ) ;
#16924 = DIRECTION ( 'NONE',  ( 1.000000000000000000, 0.000000000000000000, 8.673617379884037937E-17 ) ) ;
#16925 = DIRECTION ( 'NONE',  ( 0.000000000000000000, -0.000000000000000000, 1.000000000000000000 ) ) ;
#16926 = CARTESIAN_POINT ( 'NONE',  ( -22.80699178664539772, 18.00000000000000000, 18.33022619056923119 ) ) ;
#16927 = FACE_OUTER_BOUND ( 'NONE', #3855, .T. ) ;
#16928 = CARTESIAN_POINT ( 'NONE',  ( 29.73563295595405975, 140.6225526278764733, -16.24764948572449796 ) ) ;
#16929 = ORIENTED_EDGE ( 'NONE', *, *, #14690, .F. ) ;
#16930 = CARTESIAN_POINT ( 'NONE',  ( 196.0000000000000000, 163.6227766016838530, 15.00000337241049486 ) ) ;
#16931 = EDGE_CURVE ( 'NONE', #12800, #6747, #2276, .T. ) ;
#16932 = EDGE_LOOP ( 'NONE', ( #7862, #8319, #11170, #5422, #7536 ) ) ;
#16933 = LINE ( 'NONE', #10199, #13849 ) ;
#16934 = MANIFOLD_SOLID_BREP ( 'Hex', #17419 ) ;
#16935 = CIRCLE ( 'NONE', #13267, 19.49999999999998934 ) ;
#16936 = CARTESIAN_POINT ( 'NONE',  ( 225.0000000000000000, 89.99999999999997158, -13.00000000000000000 ) ) ;
#16937 = VECTOR ( 'NONE', #3031, 1000.000000000000000 ) ;
#16938 = EDGE_LOOP ( 'NONE', ( #6354, #12835, #7111, #633 ) ) ;
#16939 = FACE_OUTER_BOUND ( 'NONE', #15896, .T. ) ;
#16940 = VECTOR ( 'NONE', #17373, 1000.000000000000000 ) ;
#16941 = CARTESIAN_POINT ( 'NONE',  ( 25.06493225369642630, 19.99999999999999645, 5.669446505520304491 ) ) ;
#16942 = ORIENTED_EDGE ( 'NONE', *, *, #6258, .F. ) ;
#16943 = DIRECTION ( 'NONE',  ( 8.673617379884037937E-17, 0.000000000000000000, 1.000000000000000000 ) ) ;
#16944 = CARTESIAN_POINT ( 'NONE',  ( -75.00000000000000000, 196.6227766016838245, 21.54065922853802206 ) ) ;
#16945 = CIRCLE ( 'NONE', #11577, 12.00000000000000000 ) ;
#16946 = CIRCLE ( 'NONE', #1406, 20.00000000000000355 ) ;
#16947 = CARTESIAN_POINT ( 'NONE',  ( -10.71009414332545973, 30.74249144840758063, -14.53036023671900168 ) ) ;
#16948 = DIRECTION ( 'NONE',  ( 0.000000000000000000, -1.000000000000000000, -6.123233995736762338E-17 ) ) ;
#16949 = AXIS2_PLACEMENT_3D ( 'NONE', #2668, #2759, #1168 ) ;
#16950 = DIRECTION ( 'NONE',  ( 1.000000000000000000, 0.000000000000000000, 0.000000000000000000 ) ) ;
#16951 = CIRCLE ( 'NONE', #2821, 20.00000000000000355 ) ;
#16952 = ORIENTED_EDGE ( 'NONE', *, *, #7117, .F. ) ;
#16953 = DIRECTION ( 'NONE',  ( -0.000000000000000000, -0.000000000000000000, 1.000000000000000000 ) ) ;
#16954 = EDGE_CURVE ( 'NONE', #7220, #14384, #5296, .T. ) ;
#16955 = EDGE_CURVE ( 'NONE', #15131, #1074, #491, .T. ) ;
#16956 = FACE_OUTER_BOUND ( 'NONE', #16997, .T. ) ;
#16957 = ADVANCED_FACE ( 'NONE', ( #8371 ), #1395, .F. ) ;
#16958 = ORIENTED_EDGE ( 'NONE', *, *, #6993, .F. ) ;
#16959 = CARTESIAN_POINT ( 'NONE',  ( 27.59167911046515087, 191.1229741556853128, -29.06467671913508966 ) ) ;
#16960 = DIRECTION ( 'NONE',  ( 0.000000000000000000, 0.000000000000000000, 1.000000000000000000 ) ) ;
#16961 = ORIENTED_EDGE ( 'NONE', *, *, #11698, .F. ) ;
#16962 = VERTEX_POINT ( 'NONE', #12457 ) ;
#16963 = CIRCLE ( 'NONE', #1134, 25.00000000000000000 ) ;
#16964 = VECTOR ( 'NONE', #12009, 1000.000000000000000 ) ;
#16965 = VERTEX_POINT ( 'NONE', #4135 ) ;
#16966 = CARTESIAN_POINT ( 'NONE',  ( -187.6513770290094385, 171.1853623553244006, 0.7576236986490064718 ) ) ;
#16967 = AXIS2_PLACEMENT_3D ( 'NONE', #6461, #2654, #11854 ) ;
#16968 = VERTEX_POINT ( 'NONE', #17510 ) ;
#16969 = CARTESIAN_POINT ( 'NONE',  ( 27.99999999999998224, 9.999999999999998224, -28.00000000000001066 ) ) ;
#16970 = CARTESIAN_POINT ( 'NONE',  ( 15.41470791700940879, 125.6764093509959963, 6.286214449974339757 ) ) ;
#16971 = CARTESIAN_POINT ( 'NONE',  ( 40.00000000000000711, 171.6227766016838245, 0.000000000000000000 ) ) ;
#16972 = DIRECTION ( 'NONE',  ( 1.000000000000000000, 0.000000000000000000, 0.000000000000000000 ) ) ;
#16973 = VERTEX_POINT ( 'NONE', #9523 ) ;
#16974 = CARTESIAN_POINT ( 'NONE',  ( 26.92745052348471546, 139.3035600351462904, 6.678622460562388952 ) ) ;
#16975 = VECTOR ( 'NONE', #7939, 1000.000000000000000 ) ;
#16976 = AXIS2_PLACEMENT_3D ( 'NONE', #15467, #1834, #510 ) ;
#16977 = CARTESIAN_POINT ( 'NONE',  ( 49.99999999999998579, 155.6227766016839098, -12.50000337241049309 ) ) ;
#16978 = EDGE_CURVE ( 'NONE', #2044, #4758, #17457, .T. ) ;
#16979 = CARTESIAN_POINT ( 'NONE',  ( -25.00000000000000000, 120.0000000000000426, -10.85786437626905077 ) ) ;
#16980 = VECTOR ( 'NONE', #13793, 1000.000000000000000 ) ;
#16981 = CARTESIAN_POINT ( 'NONE',  ( -10.84365596476886395, 30.77158821550125722, -14.49076147631418721 ) ) ;
#16982 = CARTESIAN_POINT ( 'NONE',  ( 30.09541270076643471, 201.6232707959689208, 13.74664867617480901 ) ) ;
#16983 = ORIENTED_EDGE ( 'NONE', *, *, #7428, .F. ) ;
#16984 = CARTESIAN_POINT ( 'NONE',  ( -151.0000000000000284, 171.6227766016838245, 6.000000000000005329 ) ) ;
#16985 = AXIS2_PLACEMENT_3D ( 'NONE', #10840, #9599, #9248 ) ;
#16986 = VERTEX_POINT ( 'NONE', #1659 ) ;
#16987 = DIRECTION ( 'NONE',  ( 0.000000000000000000, -1.000000000000000000, -7.341990890863118602E-16 ) ) ;
#16988 = AXIS2_PLACEMENT_3D ( 'NONE', #3137, #15344, #7122 ) ;
#16989 = CARTESIAN_POINT ( 'NONE',  ( 22.50000000000001421, 146.6227766016838245, -35.00200000000000244 ) ) ;
#16990 = EDGE_CURVE ( 'NONE', #209, #10464, #9813, .T. ) ;
#16991 = CARTESIAN_POINT ( 'NONE',  ( 14.23753691287610579, 127.5498911642838635, -8.870798623635511859 ) ) ;
#16992 = VERTEX_POINT ( 'NONE', #14930 ) ;
#16993 = CARTESIAN_POINT ( 'NONE',  ( -80.00000000000001421, 196.6227766016838245, -16.00000000000000000 ) ) ;
#16994 = CARTESIAN_POINT ( 'NONE',  ( -103.0000000000000142, 171.6227766016838245, 0.000000000000000000 ) ) ;
#16995 = CARTESIAN_POINT ( 'NONE',  ( -151.0000000000000284, 171.6227766016838245, 0.000000000000000000 ) ) ;
#16996 = CARTESIAN_POINT ( 'NONE',  ( 33.15164470903668104, 201.7321575960915254, -17.84571802696398279 ) ) ;
#16997 = EDGE_LOOP ( 'NONE', ( #486, #11665, #15061, #12880 ) ) ;
#16998 = CIRCLE ( 'NONE', #2011, 19.49999999999999645 ) ;
#16999 = ORIENTED_EDGE ( 'NONE', *, *, #9944, .T. ) ;
#17000 = CARTESIAN_POINT ( 'NONE',  ( 17.20984524040877872, 19.99999999999999645, -14.76996962246643896 ) ) ;
#17001 = LINE ( 'NONE', #3371, #14049 ) ;
#17002 = ORIENTED_EDGE ( 'NONE', *, *, #17322, .T. ) ;
#17003 = PLANE ( 'NONE',  #9229 ) ;
#17004 = DIRECTION ( 'NONE',  ( 0.000000000000000000, 0.000000000000000000, -1.000000000000000000 ) ) ;
#17005 = ORIENTED_EDGE ( 'NONE', *, *, #7337, .T. ) ;
#17006 = DIRECTION ( 'NONE',  ( 0.000000000000000000, 1.000000000000000000, 0.000000000000000000 ) ) ;
#17007 = CIRCLE ( 'NONE', #12194, 6.000000000000005329 ) ;
#17008 = ADVANCED_FACE ( 'NONE', ( #63 ), #6986, .F. ) ;
#17009 = LINE ( 'NONE', #7697, #8678 ) ;
#17010 = CARTESIAN_POINT ( 'NONE',  ( 49.99999999999998579, 167.6227766016838530, 5.571800142134975431 ) ) ;
#17011 = CARTESIAN_POINT ( 'NONE',  ( -14.45029498972267668, 32.22448475281832003, 9.930813566224275135 ) ) ;
#17012 = FACE_OUTER_BOUND ( 'NONE', #6183, .T. ) ;
#17013 = CARTESIAN_POINT ( 'NONE',  ( 17.00000000000000000, 154.3022685259950038, -9.999999999999900524 ) ) ;
#17014 = EDGE_LOOP ( 'NONE', ( #1145, #5214, #16255 ) ) ;
#17015 = CARTESIAN_POINT ( 'NONE',  ( -103.0000000000000142, 171.6227766016838245, 5.000000000000007994 ) ) ;
#17016 = ORIENTED_EDGE ( 'NONE', *, *, #146, .T. ) ;
#17017 = EDGE_CURVE ( 'NONE', #12455, #9911, #2719, .T. ) ;
#17018 = DIRECTION ( 'NONE',  ( 0.000000000000000000, 0.000000000000000000, 1.000000000000000000 ) ) ;
#17019 = ADVANCED_FACE ( 'NONE', ( #15016 ), #11115, .F. ) ;
#17020 = DIRECTION ( 'NONE',  ( 0.000000000000000000, 1.000000000000000000, -1.224646799147353207E-16 ) ) ;
#17021 = EDGE_LOOP ( 'NONE', ( #4507, #9612, #928, #3103 ) ) ;
#17022 = DIRECTION ( 'NONE',  ( -1.000000000000000000, 0.000000000000000000, 0.000000000000000000 ) ) ;
#17023 = CARTESIAN_POINT ( 'NONE',  ( 31.20232444246483894, 19.99999999999999645, 16.65183244246150451 ) ) ;
#17024 = EDGE_LOOP ( 'NONE', ( #15488, #11553, #1175, #594 ) ) ;
#17025 = B_SPLINE_CURVE_WITH_KNOTS ( 'NONE', 3,
 ( #13814, #8395, #4074, #15214, #84, #8490, #12291, #15032, #422, #8134, #2911, #164, #5573, #344, #8300, #13904, #5829, #13713, #1584, #10870, #259, #6985, #4160, #5663, #1679, #1762, #11053, #7079, #14863, #7159, #14948, #4331, #12476, #11131, #16550, #9453, #15382, #6010, #614, #10161, #697, #6266, #1937, #4599 ),
 .UNSPECIFIED., .F., .F.,
 ( 4, 2, 2, 2, 2, 2, 2, 2, 2, 2, 2, 2, 2, 2, 2, 2, 2, 2, 2, 2, 2, 4 ),
 ( 0.000000000000000000, 0.002715240924237333209, 0.003394051155296675618, 0.004072861386356018028, 0.005430481848474658611, 0.006788102310593301797, 0.008145722772711942380, 0.009503343234830586433, 0.01018215346588990759, 0.01086096369694922875, 0.01153977392800854991, 0.01221858415906786934, 0.01289739439012719223, 0.01357620462118651339, 0.01493382508330519561, 0.01629144554542387782, 0.01697025577648323194, 0.01764906600754258606, 0.01900668646966127348, 0.01968549670072059291, 0.02036430693177990886, 0.02172192739389853383 ),
 .UNSPECIFIED. ) ;
#17026 = DIRECTION ( 'NONE',  ( 0.000000000000000000, 0.000000000000000000, -1.000000000000000000 ) ) ;
#17027 = DIRECTION ( 'NONE',  ( 0.000000000000000000, 0.000000000000000000, 1.000000000000000000 ) ) ;
#17028 = CARTESIAN_POINT ( 'NONE',  ( 196.0000000000000000, 151.6227766016839098, -3.071800142134974099 ) ) ;
#17029 = CARTESIAN_POINT ( 'NONE',  ( -9.392228533940972568, 30.65825049985634010, -12.80200153553487752 ) ) ;
#17030 = ORIENTED_EDGE ( 'NONE', *, *, #10851, .F. ) ;
#17031 = DIRECTION ( 'NONE',  ( -1.000000000000000000, 0.000000000000000000, 0.000000000000000000 ) ) ;
#17032 = CARTESIAN_POINT ( 'NONE',  ( -17.58288004918492931, 20.00000000000000355, -22.43027208364174285 ) ) ;
#17033 = ORIENTED_EDGE ( 'NONE', *, *, #11009, .F. ) ;
#17034 = CARTESIAN_POINT ( 'NONE',  ( 35.90059120242804624, 195.3277913626825466, -25.76530748039452590 ) ) ;
#17035 = CARTESIAN_POINT ( 'NONE',  ( 39.99999999999998579, 8.000000000000007105, 30.00000000000001066 ) ) ;
#17036 = ORIENTED_EDGE ( 'NONE', *, *, #4250, .T. ) ;
#17037 = ORIENTED_EDGE ( 'NONE', *, *, #250, .F. ) ;
#17038 = ORIENTED_EDGE ( 'NONE', *, *, #12920, .F. ) ;
#17039 = CARTESIAN_POINT ( 'NONE',  ( -72.50000000000002842, 146.6227766016838245, -21.54065922853802562 ) ) ;
#17040 = ORIENTED_EDGE ( 'NONE', *, *, #3787, .F. ) ;
#17041 = PRESENTATION_STYLE_ASSIGNMENT (( #14554 ) ) ;
#17042 = EDGE_CURVE ( 'NONE', #1250, #2797, #6431, .T. ) ;
#17043 = DIRECTION ( 'NONE',  ( -1.000000000000000000, -0.000000000000000000, 0.000000000000000000 ) ) ;
#17044 = LINE ( 'NONE', #4911, #6941 ) ;
#17045 = CARTESIAN_POINT ( 'NONE',  ( 35.27494917608787972, 141.2912748254776147, -13.00000000000000000 ) ) ;
#17046 = CARTESIAN_POINT ( 'NONE',  ( 34.93420767853318409, 18.00000000000000000, 5.000000000000010658 ) ) ;
#17047 = CARTESIAN_POINT ( 'NONE',  ( 35.49999999999998579, 9.999999999999998224, -13.00000000000000000 ) ) ;
#17048 = ORIENTED_EDGE ( 'NONE', *, *, #11403, .F. ) ;
#17049 = CARTESIAN_POINT ( 'NONE',  ( 22.64347415271929265, 141.1870565414818941, 12.76399958404563684 ) ) ;
#17050 = CARTESIAN_POINT ( 'NONE',  ( -24.93725393319379435, 120.0000000000000284, -5.500000000000000000 ) ) ;
#17051 = FACE_OUTER_BOUND ( 'NONE', #14644, .T. ) ;
#17052 = CARTESIAN_POINT ( 'NONE',  ( 39.99999999999998579, 4.000000000000000000, -30.00000000000000000 ) ) ;
#17053 = LINE ( 'NONE', #3513, #7225 ) ;
#17054 = CARTESIAN_POINT ( 'NONE',  ( 27.75123839167244810, 201.0919203481101079, 14.85271610579516555 ) ) ;
#17055 = VERTEX_POINT ( 'NONE', #16526 ) ;
#17056 = CARTESIAN_POINT ( 'NONE',  ( 49.99999999999998579, 155.6227766016839098, 15.00000337241049486 ) ) ;
#17057 = DIRECTION ( 'NONE',  ( 0.000000000000000000, 0.000000000000000000, -1.000000000000000000 ) ) ;
#17058 = EDGE_LOOP ( 'NONE', ( #9448, #16620, #13318, #9343 ) ) ;
#17059 = ADVANCED_FACE ( 'NONE', ( #9613 ), #1302, .T. ) ;
#17060 = EDGE_CURVE ( 'NONE', #554, #2291, #1559, .T. ) ;
#17061 = CARTESIAN_POINT ( 'NONE',  ( -75.21246548080814875, 145.1525832006840346, 19.71138291685208799 ) ) ;
#17062 = EDGE_CURVE ( 'NONE', #11495, #17220, #236, .T. ) ;
#17063 = ADVANCED_FACE ( 'NONE', ( #4315 ), #9694, .F. ) ;
#17064 = CARTESIAN_POINT ( 'NONE',  ( -16.40540729975244716, 18.00000000000000000, 23.03124090058167184 ) ) ;
#17065 = DIRECTION ( 'NONE',  ( 0.000000000000000000, 1.000000000000000000, 0.000000000000000000 ) ) ;
#17066 = MANIFOLD_SOLID_BREP ( '<Left Housing Shell>-<Boss-Extrude6>', #16856 ) ;
#17067 = CARTESIAN_POINT ( 'NONE',  ( 30.00000000000000355, 196.6227766016838245, -16.00000000000000000 ) ) ;
#17068 = ORIENTED_EDGE ( 'NONE', *, *, #2520, .F. ) ;
#17069 = CARTESIAN_POINT ( 'NONE',  ( 15.39006516123636281, 143.0404737187717785, 16.50200026350847793 ) ) ;
#17070 = DIRECTION ( 'NONE',  ( 1.000000000000000000, 0.000000000000000000, 0.000000000000000000 ) ) ;
#17071 = CARTESIAN_POINT ( 'NONE',  ( -168.3486229709906183, 166.3256969276982886, -9.174811127083483342 ) ) ;
#17072 = ORIENTED_EDGE ( 'NONE', *, *, #10012, .F. ) ;
#17073 = SHAPE_REPRESENTATION ( 'Detachable Battery Pack Module', ( #3583 ), #803 ) ;
#17074 = ORIENTED_EDGE ( 'NONE', *, *, #5921, .F. ) ;
#17075 = CARTESIAN_POINT ( 'NONE',  ( 16.23563086566769442, 20.00000000000456879, -14.95434718295347665 ) ) ;
#17076 = VECTOR ( 'NONE', #10693, 1000.000000000000000 ) ;
#17077 = CARTESIAN_POINT ( 'NONE',  ( 11.08062248138317685, 138.8595139650515193, -13.56485289975001862 ) ) ;
#17078 = ORIENTED_EDGE ( 'NONE', *, *, #9845, .T. ) ;
#17079 = EDGE_CURVE ( 'NONE', #9609, #5427, #5014, .T. ) ;
#17080 = CARTESIAN_POINT ( 'NONE',  ( -997.5739745962155212, 0.000000000000000000, 0.000000000000000000 ) ) ;
#17081 = CARTESIAN_POINT ( 'NONE',  ( -2.428612866367531510E-15, 2.000000000000000000, 28.00000000000000711 ) ) ;
#17082 = EDGE_LOOP ( 'NONE', ( #14107, #749, #16229, #17333 ) ) ;
#17083 = CARTESIAN_POINT ( 'NONE',  ( 30.00000000000000355, 196.6227766016838245, -35.00200000000000244 ) ) ;
#17084 = CARTESIAN_POINT ( 'NONE',  ( -197.9999999999999716, 171.6227766016838245, -14.16444493696511486 ) ) ;
#17085 = VECTOR ( 'NONE', #7274, 1000.000000000000000 ) ;
#17086 = DIRECTION ( 'NONE',  ( 0.000000000000000000, 1.000000000000000000, 0.000000000000000000 ) ) ;
#17087 = CARTESIAN_POINT ( 'NONE',  ( -7.965954974912850872, 30.19485118722929329, 13.00000000000000178 ) ) ;
#17088 = AXIS2_PLACEMENT_3D ( 'NONE', #3644, #17090, #3552 ) ;
#17089 = DIRECTION ( 'NONE',  ( -1.000000000000000000, 0.000000000000000000, 0.000000000000000000 ) ) ;
#17090 = DIRECTION ( 'NONE',  ( -1.000000000000000000, -0.000000000000000000, 0.000000000000000000 ) ) ;
#17091 = VERTEX_POINT ( 'NONE', #8468 ) ;
#17092 = FACE_OUTER_BOUND ( 'NONE', #1005, .T. ) ;
#17093 = EDGE_LOOP ( 'NONE', ( #14193, #13831, #5783 ) ) ;
#17094 = CARTESIAN_POINT ( 'NONE',  ( 30.00000000000000355, 196.6227766016838245, 1.387778780781445676E-14 ) ) ;
#17095 = FACE_OUTER_BOUND ( 'NONE', #15443, .T. ) ;
#17096 = ADVANCED_FACE ( 'NONE', ( #6158 ), #5023, .F. ) ;
#17097 = ORIENTED_EDGE ( 'NONE', *, *, #10920, .F. ) ;
#17098 = EDGE_CURVE ( 'NONE', #9987, #2414, #11789, .T. ) ;
#17099 = CARTESIAN_POINT ( 'NONE',  ( 33.66231827095856488, 20.00000000000000000, 12.04861179558545636 ) ) ;
#17100 = DIRECTION ( 'NONE',  ( 0.000000000000000000, 0.000000000000000000, 1.000000000000000000 ) ) ;
#17101 = AXIS2_PLACEMENT_3D ( 'NONE', #3021, #4540, #15504 ) ;
#17102 = PRESENTATION_LAYER_ASSIGNMENT (  '', '', ( #11453 ) ) ;
#17103 = CARTESIAN_POINT ( 'NONE',  ( 23.15530394309853435, 20.00000000000112976, 10.88800651875285297 ) ) ;
#17104 = ORIENTED_EDGE ( 'NONE', *, *, #7097, .T. ) ;
#17105 = DIRECTION ( 'NONE',  ( 0.000000000000000000, 0.000000000000000000, 1.000000000000000000 ) ) ;
#17106 = ADVANCED_FACE ( 'NONE', ( #4490 ), #15362, .F. ) ;
#17107 = CARTESIAN_POINT ( 'NONE',  ( 27.18614160573789817, 189.6648409365396049, -27.63145166803555242 ) ) ;
#17108 = CARTESIAN_POINT ( 'NONE',  ( 20.49999999999998224, 10.00000000000000000, -28.00000000000001066 ) ) ;
#17109 = CARTESIAN_POINT ( 'NONE',  ( -19.26597175465492739, 18.00000000000000000, -21.35691006828201566 ) ) ;
#17110 = COLOUR_RGB ( '', 0.09019608, 0.27058824, 0.51372549) ;
#17111 = ORIENTED_EDGE ( 'NONE', *, *, #10282, .T. ) ;
#17112 = DIRECTION ( 'NONE',  ( 1.000000000000000000, 0.000000000000000000, 0.000000000000000000 ) ) ;
#17113 = CIRCLE ( 'NONE', #17411, 5.000000000000004441 ) ;
#17114 = ORIENTED_EDGE ( 'NONE', *, *, #624, .F. ) ;
#17115 = CYLINDRICAL_SURFACE ( 'NONE', #12700, 2.500000000000000444 ) ;
#17116 = DIRECTION ( 'NONE',  ( -1.000000000000000000, 0.000000000000000000, 0.000000000000000000 ) ) ;
#17117 = ORIENTED_EDGE ( 'NONE', *, *, #15448, .F. ) ;
#17118 = ORIENTED_EDGE ( 'NONE', *, *, #8606, .F. ) ;
#17119 = ORIENTED_EDGE ( 'NONE', *, *, #8283, .F. ) ;
#17120 = CARTESIAN_POINT ( 'NONE',  ( -77.18614160573793015, 153.5807122668280442, -27.63145166803555952 ) ) ;
#17121 = ORIENTED_EDGE ( 'NONE', *, *, #16359, .F. ) ;
#17122 = DIRECTION ( 'NONE',  ( 1.000000000000000000, 0.000000000000000000, 0.000000000000000000 ) ) ;
#17123 = DIRECTION ( 'NONE',  ( -0.000000000000000000, -0.000000000000000000, -1.000000000000000000 ) ) ;
#17124 = CIRCLE ( 'NONE', #4427, 5.000000000000000888 ) ;
#17125 = CARTESIAN_POINT ( 'NONE',  ( -10.05507621332305668, 30.59909908010286372, 14.70163937327580328 ) ) ;
#17126 = EDGE_CURVE ( 'NONE', #13808, #3225, #15455, .T. ) ;
#17127 = CARTESIAN_POINT ( 'NONE',  ( 30.00000000000001066, 146.6227766016838245, 10.00000000000000178 ) ) ;
#17128 = CARTESIAN_POINT ( 'NONE',  ( 22.81311145407750374, 18.00000000000113687, 7.108351238697862229 ) ) ;
#17129 = DIRECTION ( 'NONE',  ( -0.08715574274764661955, -0.4980973490458647235, -0.8627299156628267518 ) ) ;
#17130 = ORIENTED_EDGE ( 'NONE', *, *, #17079, .F. ) ;
#17131 = DIRECTION ( 'NONE',  ( -1.000000000000000000, 0.000000000000000000, 0.000000000000000000 ) ) ;
#17132 = CARTESIAN_POINT ( 'NONE',  ( -32.93725393319379435, 120.0000000000000284, -5.500000000000000000 ) ) ;
#17133 = CARTESIAN_POINT ( 'NONE',  ( 125.0000000000000000, 0.000000000000000000, 0.000000000000000000 ) ) ;
#17134 = LINE ( 'NONE', #11650, #16374 ) ;
#17135 = VERTEX_POINT ( 'NONE', #10136 ) ;
#17136 = FACE_OUTER_BOUND ( 'NONE', #3499, .T. ) ;
#17137 = AXIS2_PLACEMENT_3D ( 'NONE', #9936, #4633, #12776 ) ;
#17138 = EDGE_CURVE ( 'NONE', #13884, #17055, #673, .T. ) ;
#17139 = VECTOR ( 'NONE', #2778, 1000.000000000000000 ) ;
#17140 = CARTESIAN_POINT ( 'NONE',  ( 25.40795165748616569, 198.6215000397447739, 18.98099903503497288 ) ) ;
#17141 = ORIENTED_EDGE ( 'NONE', *, *, #13054, .F. ) ;
#17142 = CARTESIAN_POINT ( 'NONE',  ( 27.99999999999998224, 9.999999999999998224, 0.000000000000000000 ) ) ;
#17143 = DIRECTION ( 'NONE',  ( 1.000000000000000000, 0.000000000000000000, 0.000000000000000000 ) ) ;
#17144 = ORIENTED_EDGE ( 'NONE', *, *, #13103, .F. ) ;
#17145 = LINE ( 'NONE', #10506, #12734 ) ;
#17147 = CARTESIAN_POINT ( 'NONE',  ( -153.0000000000000284, 171.6227766016838245, -23.57392898041431195 ) ) ;
#17146 = CIRCLE ( 'NONE', #467, 7.499999999999996447 ) ;
#17148 = CARTESIAN_POINT ( 'NONE',  ( -78.00663513009409655, 140.9591509882842786, -16.87514788462641491 ) ) ;
#17149 = VECTOR ( 'NONE', #15308, 1000.000000000000000 ) ;
#17150 =( GEOMETRIC_REPRESENTATION_CONTEXT ( 3 ) GLOBAL_UNCERTAINTY_ASSIGNED_CONTEXT ( ( #635 ) ) GLOBAL_UNIT_ASSIGNED_CONTEXT ( ( #4493, #6161, #12885 ) ) REPRESENTATION_CONTEXT ( 'NONE', 'WORKASPACE' ) );
#17151 = CARTESIAN_POINT ( 'NONE',  ( 15.04007972439966956, 126.3543340278276190, -7.435061541642935978 ) ) ;
#17152 = AXIS2_PLACEMENT_3D ( 'NONE', #1759, #8296, #15029 ) ;
#17153 = ORIENTED_EDGE ( 'NONE', *, *, #1226, .F. ) ;
#17154 = LINE ( 'NONE', #1220, #16323 ) ;
#17155 = CARTESIAN_POINT ( 'NONE',  ( 13.57836111649853450, 143.5532840108684525, 17.35359164609418059 ) ) ;
#17156 = CARTESIAN_POINT ( 'NONE',  ( -73.00000000000001421, 171.6227766016838245, 0.000000000000000000 ) ) ;
#17157 = CARTESIAN_POINT ( 'NONE',  ( 28.71601389420674622, 202.4851391218125798, -16.50809708901796213 ) ) ;
#17158 = ORIENTED_EDGE ( 'NONE', *, *, #5353, .T. ) ;
#17159 = EDGE_CURVE ( 'NONE', #1460, #15793, #11639, .T. ) ;
#17160 = EDGE_CURVE ( 'NONE', #7936, #13265, #10961, .T. ) ;
#17161 = ADVANCED_FACE ( 'NONE', ( #12719 ), #11554, .F. ) ;
#17162 = ORIENTED_EDGE ( 'NONE', *, *, #3422, .T. ) ;
#17163 = CARTESIAN_POINT ( 'NONE',  ( -80.00000000000002842, 146.6227766016838245, -35.00200000000000244 ) ) ;
#17164 = ORIENTED_EDGE ( 'NONE', *, *, #15621, .T. ) ;
#17165 = CARTESIAN_POINT ( 'NONE',  ( 11.61835878478676598, 131.7755375868723320, -13.65455057792075877 ) ) ;
#17166 = VECTOR ( 'NONE', #9983, 1000.000000000000000 ) ;
#17167 = ORIENTED_EDGE ( 'NONE', *, *, #12849, .T. ) ;
#17168 = FACE_OUTER_BOUND ( 'NONE', #9559, .T. ) ;
#17169 = AXIS2_PLACEMENT_3D ( 'NONE', #13430, #9433, #14837 ) ;
#17170 = CARTESIAN_POINT ( 'NONE',  ( 26.46962346220079709, 139.5657242622003480, -7.835998493359402239 ) ) ;
#17171 = ORIENTED_EDGE ( 'NONE', *, *, #4924, .F. ) ;
#17172 = DIRECTION ( 'NONE',  ( 1.000000000000000000, 0.000000000000000000, 0.000000000000000000 ) ) ;
#17173 = DIRECTION ( 'NONE',  ( -1.000000000000000000, -0.000000000000000000, -0.000000000000000000 ) ) ;
#17174 = CARTESIAN_POINT ( 'NONE',  ( 22.79003115184357497, 198.7539484232960945, -18.80562413441370850 ) ) ;
#17175 = CARTESIAN_POINT ( 'NONE',  ( -95.00000000000000000, 171.6227766016838245, 30.00000000000000000 ) ) ;
#17176 = LINE ( 'NONE', #7879, #2444 ) ;
#17177 = DIRECTION ( 'NONE',  ( -1.000000000000000000, 0.000000000000000000, 0.000000000000000000 ) ) ;
#17178 = CARTESIAN_POINT ( 'NONE',  ( -12.63209758636676305, 18.00000000000116174, 7.167151760391626603 ) ) ;
#17179 = AXIS2_PLACEMENT_3D ( 'NONE', #11647, #7661, #13070 ) ;
#17180 = CYLINDRICAL_SURFACE ( 'NONE', #9173, 27.69059892324149530 ) ;
#17181 = CIRCLE ( 'NONE', #8976, 2.499999999999998668 ) ;
#17182 = CARTESIAN_POINT ( 'NONE',  ( 34.93420767853318409, 30.00000000000000000, 5.000000000000010658 ) ) ;
#17183 = ORIENTED_EDGE ( 'NONE', *, *, #1979, .F. ) ;
#17184 = DIRECTION ( 'NONE',  ( -1.000000000000000000, -0.000000000000000000, -0.000000000000000000 ) ) ;
#17185 = ORIENTED_EDGE ( 'NONE', *, *, #11902, .T. ) ;
#17186 = CYLINDRICAL_SURFACE ( 'NONE', #12990, 7.500000000000000000 ) ;
#17187 = DIRECTION ( 'NONE',  ( 0.000000000000000000, 0.000000000000000000, 1.000000000000000000 ) ) ;
#17188 = EDGE_LOOP ( 'NONE', ( #10081, #2007, #10849, #12073 ) ) ;
#17189 = CARTESIAN_POINT ( 'NONE',  ( -13.95500183466744382, 31.43484250012364001, 12.98634364776042638 ) ) ;
#17190 = CARTESIAN_POINT ( 'NONE',  ( 14.16484689353800697, 138.6662281288708982, 3.797024489650498325 ) ) ;
#17191 = VECTOR ( 'NONE', #4984, 1000.000000000000000 ) ;
#17192 = CARTESIAN_POINT ( 'NONE',  ( 17.53130567297317910, 19.99999999999999289, 14.69383831151754727 ) ) ;
#17193 = VERTEX_POINT ( 'NONE', #15542 ) ;
#17194 = CARTESIAN_POINT ( 'NONE',  ( 14.93242934743711992, 20.00000000000000000, -25.00000000000000000 ) ) ;
#17195 = CARTESIAN_POINT ( 'NONE',  ( 23.01962815379005178, 193.8465113367682591, -24.40116746791568758 ) ) ;
#17196 = CARTESIAN_POINT ( 'NONE',  ( -18.15427578192114666, 32.28835078156378557, -6.388283290543781412 ) ) ;
#17197 = CARTESIAN_POINT ( 'NONE',  ( -12.35971836118926959, 18.00000000000000000, -8.238707107740440350 ) ) ;
#17198 = EDGE_CURVE ( 'NONE', #7583, #1100, #788, .T. ) ;
#17199 = EDGE_LOOP ( 'NONE', ( #9809, #12228 ) ) ;
#17200 = PLANE ( 'NONE',  #12672 ) ;
#17201 = CIRCLE ( 'NONE', #16922, 2.500000000000000000 ) ;
#17202 = ORIENTED_EDGE ( 'NONE', *, *, #14003, .F. ) ;
#17203 = CARTESIAN_POINT ( 'NONE',  ( 24.00000000000000000, 196.6227766016838245, -24.49489742783178770 ) ) ;
#17204 = CIRCLE ( 'NONE', #9569, 2.500000000000000000 ) ;
#17205 = DIRECTION ( 'NONE',  ( 1.000000000000000000, -0.000000000000000000, 0.000000000000000000 ) ) ;
#17206 = ORIENTED_EDGE ( 'NONE', *, *, #13661, .F. ) ;
#17207 = ORIENTED_EDGE ( 'NONE', *, *, #6293, .F. ) ;
#17208 = ORIENTED_EDGE ( 'NONE', *, *, #9328, .T. ) ;
#17209 = LINE ( 'NONE', #2521, #5587 ) ;
#17210 = VECTOR ( 'NONE', #16663, 1000.000000000000000 ) ;
#17211 = ORIENTED_EDGE ( 'NONE', *, *, #10692, .T. ) ;
#17212 = DIRECTION ( 'NONE',  ( 1.000000000000000000, 0.000000000000000000, 0.000000000000000000 ) ) ;
#17213 = CIRCLE ( 'NONE', #3081, 2.500000000000002220 ) ;
#17214 = DIRECTION ( 'NONE',  ( -0.000000000000000000, -0.000000000000000000, -1.000000000000000000 ) ) ;
#17215 = CARTESIAN_POINT ( 'NONE',  ( 27.50000000000000355, 196.6227766016838245, -16.00000000000000000 ) ) ;
#17216 = CARTESIAN_POINT ( 'NONE',  ( 34.01748795107550905, 151.0988115558745051, -28.35253695364550452 ) ) ;
#17217 = CARTESIAN_POINT ( 'NONE',  ( 21.99569976772868074, 17.99999999999999645, 9.076888812463767664 ) ) ;
#17218 = CARTESIAN_POINT ( 'NONE',  ( -84.69896753943838519, 148.3373224442695175, 23.38426449892924452 ) ) ;
#17219 = EDGE_CURVE ( 'NONE', #6275, #16623, #10385, .T. ) ;
#17220 = VERTEX_POINT ( 'NONE', #3336 ) ;
#17221 = FACE_OUTER_BOUND ( 'NONE', #11510, .T. ) ;
#17222 = DIRECTION ( 'NONE',  ( -0.000000000000000000, -0.000000000000000000, -1.000000000000000000 ) ) ;
#17223 = FACE_OUTER_BOUND ( 'NONE', #12532, .T. ) ;
#17224 = DIRECTION ( 'NONE',  ( 0.000000000000000000, 0.000000000000000000, -1.000000000000000000 ) ) ;
#17225 = FACE_OUTER_BOUND ( 'NONE', #14918, .T. ) ;
#17226 = ORIENTED_EDGE ( 'NONE', *, *, #13026, .F. ) ;
#17227 = CARTESIAN_POINT ( 'NONE',  ( 24.72505082391212028, 201.9542783778900059, -13.00000000000000000 ) ) ;
#17228 = VECTOR ( 'NONE', #3169, 1000.000000000000000 ) ;
#17229 = EDGE_CURVE ( 'NONE', #15578, #1044, #2475, .T. ) ;
#17230 = AXIS2_PLACEMENT_3D ( 'NONE', #5420, #4175, #3819 ) ;
#17231 = EDGE_CURVE ( 'NONE', #8971, #1773, #1306, .T. ) ;
#17232 = AXIS2_PLACEMENT_3D ( 'NONE', #11417, #1873, #8850 ) ;
#17233 = ADVANCED_FACE ( 'NONE', ( #6504 ), #15971, .T. ) ;
#17234 = CARTESIAN_POINT ( 'NONE',  ( 25.11100433194186721, 197.8164829328480607, 20.09296681051159439 ) ) ;
#17235 = ORIENTED_EDGE ( 'NONE', *, *, #3820, .F. ) ;
#17236 = CARTESIAN_POINT ( 'NONE',  ( -32.34996859905194810, 100.2591029109095189, -5.378151393592372820 ) ) ;
#17237 = DIRECTION ( 'NONE',  ( 0.000000000000000000, 1.000000000000000000, 0.000000000000000000 ) ) ;
#17238 = ORIENTED_EDGE ( 'NONE', *, *, #1619, .T. ) ;
#17239 = SURFACE_STYLE_FILL_AREA ( #6535 ) ;
#17240 = CARTESIAN_POINT ( 'NONE',  ( -81.54154366038537205, 141.8618947663538279, 14.25856086977511339 ) ) ;
#17241 = CARTESIAN_POINT ( 'NONE',  ( -23.00000000000001421, 122.0000000000000284, -4.999999999999999112 ) ) ;
#17242 = AXIS2_PLACEMENT_3D ( 'NONE', #10773, #14835, #1299 ) ;
#17243 = LINE ( 'NONE', #5118, #7318 ) ;
#17244 = AXIS2_PLACEMENT_3D ( 'NONE', #92, #8054, #4083 ) ;
#17245 = AXIS2_PLACEMENT_3D ( 'NONE', #7360, #3545, #7267 ) ;
#17246 = DIRECTION ( 'NONE',  ( 1.000000000000000000, 0.000000000000000000, 0.000000000000000000 ) ) ;
#17247 = ORIENTED_EDGE ( 'NONE', *, *, #7335, .F. ) ;
#17248 = DIRECTION ( 'NONE',  ( 0.000000000000000000, 0.000000000000000000, -1.000000000000000000 ) ) ;
#17249 = CARTESIAN_POINT ( 'NONE',  ( -208.1243352336975079, 172.5999688864191910, -5.796121406182466629 ) ) ;
#17250 = LINE ( 'NONE', #7858, #1694 ) ;
#17251 = DIRECTION ( 'NONE',  ( 1.000000000000000000, 0.000000000000000000, 0.000000000000000000 ) ) ;
#17252 = ORIENTED_EDGE ( 'NONE', *, *, #14369, .T. ) ;
#17253 = VERTEX_POINT ( 'NONE', #14649 ) ;
#17254 = AXIS2_PLACEMENT_3D ( 'NONE', #10400, #15811, #9076 ) ;
#17255 = CARTESIAN_POINT ( 'NONE',  ( 13.85534145189689248, 141.7971685630157879, -18.31519266891907094 ) ) ;
#17256 = EDGE_LOOP ( 'NONE', ( #7188, #15064 ) ) ;
#17257 = CARTESIAN_POINT ( 'NONE',  ( 24.00000000000000355, 146.6227766016838245, -24.49489742783179480 ) ) ;
#17258 = VECTOR ( 'NONE', #7316, 1000.000000000000000 ) ;
#17259 = CARTESIAN_POINT ( 'NONE',  ( 9.466951579747838963, 140.2095812714875080, -12.14773935231208313 ) ) ;
#17260 = ORIENTED_EDGE ( 'NONE', *, *, #6807, .F. ) ;
#17261 = CYLINDRICAL_SURFACE ( 'NONE', #12370, 10.00000000000000178 ) ;
#17262 = LINE ( 'NONE', #1061, #3680 ) ;
#17263 = CARTESIAN_POINT ( 'NONE',  ( 23.58001751434002813, 200.5275637277235887, -15.94334347237690075 ) ) ;
#17264 = EDGE_CURVE ( 'NONE', #7796, #3840, #17209, .T. ) ;
#17265 = EDGE_CURVE ( 'NONE', #9474, #16675, #12972, .T. ) ;
#17266 = EDGE_CURVE ( 'NONE', #17478, #15620, #10483, .T. ) ;
#17267 = CARTESIAN_POINT ( 'NONE',  ( 33.28260143222578904, 192.8472041258102934, 25.26942977006888569 ) ) ;
#17268 = LINE ( 'NONE', #8933, #10915 ) ;
#17269 = CARTESIAN_POINT ( 'NONE',  ( -43.00000000000000711, 130.0000000000000000, -12.99999999999999822 ) ) ;
#17270 = CARTESIAN_POINT ( 'NONE',  ( -68.00000000000000000, 171.6227766016838245, 20.00000000000000355 ) ) ;
#17271 = VECTOR ( 'NONE', #12410, 1000.000000000000000 ) ;
#17272 = DIRECTION ( 'NONE',  ( -1.000000000000000000, -0.000000000000000000, 0.000000000000000000 ) ) ;
#17273 = CARTESIAN_POINT ( 'NONE',  ( -40.85786437626905609, 120.0000000000000142, -10.85786437626904721 ) ) ;
#17274 = CARTESIAN_POINT ( 'NONE',  ( 31.30883960485276418, 140.7623173628079485, -16.51208758287211253 ) ) ;
#17275 = ORIENTED_EDGE ( 'NONE', *, *, #10404, .F. ) ;
#17276 = LINE ( 'NONE', #5328, #10125 ) ;
#17277 = ORIENTED_EDGE ( 'NONE', *, *, #5450, .F. ) ;
#17278 = DIRECTION ( 'NONE',  ( 0.000000000000000000, 0.000000000000000000, 1.000000000000000000 ) ) ;
#17279 = CARTESIAN_POINT ( 'NONE',  ( -96.00000000000001421, 171.6227766016838245, 0.000000000000000000 ) ) ;
#17280 = ORIENTED_EDGE ( 'NONE', *, *, #2680, .F. ) ;
#17281 = FACE_OUTER_BOUND ( 'NONE', #14133, .T. ) ;
#17282 = CARTESIAN_POINT ( 'NONE',  ( 14.92136712345229554, 126.5341449364669728, 7.654582290614115436 ) ) ;
#17283 = TOROIDAL_SURFACE ( 'NONE', #4006, 240.0000000000000000, 10.00000000000000000 ) ;
#17284 = ORIENTED_EDGE ( 'NONE', *, *, #13206, .T. ) ;
#17285 = CARTESIAN_POINT ( 'NONE',  ( 15.58496356726128873, 29.99118438505512430, 15.00000000000000000 ) ) ;
#17286 = VERTEX_POINT ( 'NONE', #5443 ) ;
#17287 = EDGE_CURVE ( 'NONE', #6948, #2358, #7564, .T. ) ;
#17288 = EDGE_CURVE ( 'NONE', #13094, #15022, #16054, .T. ) ;
#17289 = ADVANCED_FACE ( 'NONE', ( #2615 ), #8086, .T. ) ;
#17290 = EDGE_CURVE ( 'NONE', #16339, #5589, #13672, .T. ) ;
#17291 = DIRECTION ( 'NONE',  ( 1.000000000000000000, 0.000000000000000000, 0.000000000000000000 ) ) ;
#17292 = CARTESIAN_POINT ( 'NONE',  ( -34.99999999999999289, 122.0000000000000284, -15.00000000000000000 ) ) ;
#17293 = CARTESIAN_POINT ( 'NONE',  ( 196.0000000000000000, 151.6227766016839098, -5.571800142134973655 ) ) ;
#17294 = CARTESIAN_POINT ( 'NONE',  ( -12.55890155933072094, 17.99999999999999645, -7.515612101507581855 ) ) ;
#17295 = EDGE_LOOP ( 'NONE', ( #7402, #764, #7169, #2404, #178, #5741 ) ) ;
#17296 = CARTESIAN_POINT ( 'NONE',  ( -80.00000000000002842, 146.6227766016838245, -35.00200000000000244 ) ) ;
#17297 = VERTEX_POINT ( 'NONE', #10833 ) ;
#17298 = FACE_OUTER_BOUND ( 'NONE', #14011, .T. ) ;
#17299 = CARTESIAN_POINT ( 'NONE',  ( -86.65363293176820036, 200.1176944260899688, -16.66575456205189809 ) ) ;
#17300 = ORIENTED_EDGE ( 'NONE', *, *, #4788, .F. ) ;
#17301 = EDGE_LOOP ( 'NONE', ( #13416, #12683 ) ) ;
#17302 = ORIENTED_EDGE ( 'NONE', *, *, #394, .F. ) ;
#17303 = EDGE_CURVE ( 'NONE', #4748, #4908, #10948, .T. ) ;
#17304 = CARTESIAN_POINT ( 'NONE',  ( -85.08450508553750069, 152.1614365523548713, -26.65369102675423463 ) ) ;
#17305 = UNCERTAINTY_MEASURE_WITH_UNIT (LENGTH_MEASURE( 1.000000000000000082E-05 ), #11826, 'distance_accuracy_value', 'NONE');
#17306 = EDGE_LOOP ( 'NONE', ( #12141, #6726, #1975, #14804 ) ) ;
#17307 = SURFACE_SIDE_STYLE ('',( #6245 ) ) ;
#17308 = CARTESIAN_POINT ( 'NONE',  ( -15.27350142870561811, 32.46802521863179436, 8.792838265516087048 ) ) ;
#17309 = CARTESIAN_POINT ( 'NONE',  ( -7.379000772444994638, 30.00000000000000000, 15.00000000000000000 ) ) ;
#17310 = CARTESIAN_POINT ( 'NONE',  ( 24.58837873217347081, 149.2402085794911955, -26.91083197558416629 ) ) ;
#17311 = CARTESIAN_POINT ( 'NONE',  ( 28.14717441101696593, 18.00000000000000000, 20.07001214884044415 ) ) ;
#17312 = CARTESIAN_POINT ( 'NONE',  ( -84.07431145984972432, 149.5391923287904490, 24.52402115671404204 ) ) ;
#17313 = ORIENTED_EDGE ( 'NONE', *, *, #16579, .T. ) ;
#17314 = FACE_OUTER_BOUND ( 'NONE', #11620, .T. ) ;
#17315 = DIRECTION ( 'NONE',  ( 0.000000000000000000, -0.000000000000000000, -1.000000000000000000 ) ) ;
#17316 = CARTESIAN_POINT ( 'NONE',  ( 10.11940563665161541, 132.7319563576625399, 14.29042643364863885 ) ) ;
#17317 = CARTESIAN_POINT ( 'NONE',  ( -15.18548748502429468, 20.00000000000231992, -6.873064813191830602 ) ) ;
#17318 = VERTEX_POINT ( 'NONE', #2697 ) ;
#17319 = LINE ( 'NONE', #12101, #6367 ) ;
#17320 = CARTESIAN_POINT ( 'NONE',  ( 34.89002926043553288, 197.8146641845671923, 20.09570409464927465 ) ) ;
#17321 = ORIENTED_EDGE ( 'NONE', *, *, #3814, .F. ) ;
#17322 = EDGE_CURVE ( 'NONE', #3758, #10541, #12102, .T. ) ;
#17323 = DIRECTION ( 'NONE',  ( -1.000000000000000000, 0.000000000000000000, -8.673617379884037937E-17 ) ) ;
#17324 = CARTESIAN_POINT ( 'NONE',  ( -43.00000000000000000, 140.0000000000000000, -13.00000000000000000 ) ) ;
#17325 = ORIENTED_EDGE ( 'NONE', *, *, #13141, .T. ) ;
#17326 =( NAMED_UNIT ( * ) SI_UNIT ( $, .STERADIAN. ) SOLID_ANGLE_UNIT ( ) );
#17327 = DIRECTION ( 'NONE',  ( 1.000000000000000000, 0.000000000000000000, 0.000000000000000000 ) ) ;
#17328 = LINE ( 'NONE', #1305, #8913 ) ;
#17329 = DIRECTION ( 'NONE',  ( 1.000000000000000000, 0.000000000000000000, -0.000000000000000000 ) ) ;
#17330 = EDGE_CURVE ( 'NONE', #16016, #11646, #16245, .T. ) ;
#17331 = CARTESIAN_POINT ( 'NONE',  ( -195.2299705378136991, 167.4686912709917124, 0.4270243643950926149 ) ) ;
#17332 = ADVANCED_FACE ( 'NONE', ( #4113 ), #15936, .F. ) ;
#17333 = ORIENTED_EDGE ( 'NONE', *, *, #6019, .F. ) ;
#17334 = CARTESIAN_POINT ( 'NONE',  ( -100.0000000000000000, 141.2912748254776147, -13.00000000000000000 ) ) ;
#17335 = DIRECTION ( 'NONE',  ( 0.000000000000000000, 0.000000000000000000, 1.000000000000000000 ) ) ;
#17336 = DIRECTION ( 'NONE',  ( 1.000000000000000000, 0.000000000000000000, 0.000000000000000000 ) ) ;
#17337 =( NAMED_UNIT ( * ) SI_UNIT ( $, .STERADIAN. ) SOLID_ANGLE_UNIT ( ) );
#17338 = ORIENTED_EDGE ( 'NONE', *, *, #14789, .T. ) ;
#17339 = ORIENTED_EDGE ( 'NONE', *, *, #7461, .F. ) ;
#17340 = CARTESIAN_POINT ( 'NONE',  ( 8.956670050029527985, 133.3372912347335841, -14.64653510947197645 ) ) ;
#17341 = VERTEX_POINT ( 'NONE', #5782 ) ;
#17342 = CARTESIAN_POINT ( 'NONE',  ( -77.79806300862335888, 152.2211730668986434, -29.13124974281949875 ) ) ;
#17343 = CARTESIAN_POINT ( 'NONE',  ( 21.84350049701177809, 141.4638053371992328, -13.40107808329819150 ) ) ;
#17344 = EDGE_LOOP ( 'NONE', ( #14358, #5187, #10587, #17388 ) ) ;
#17345 = CARTESIAN_POINT ( 'NONE',  ( -80.00000000000001421, 196.6227766016838245, 0.000000000000000000 ) ) ;
#17346 = DIRECTION ( 'NONE',  ( -1.000000000000000000, 0.000000000000000000, 0.000000000000000000 ) ) ;
#17347 = PRODUCT_DEFINITION ( 'UNKNOWN', '', #3897, #6956 ) ;
#17348 = LINE ( 'NONE', #2746, #2486 ) ;
#17349 = LINE ( 'NONE', #1063, #11490 ) ;
#17350 = CARTESIAN_POINT ( 'NONE',  ( 48.00000000000000711, 155.6227766016839098, -15.00000337241049486 ) ) ;
#17351 = ADVANCED_FACE ( 'NONE', ( #8441 ), #16592, .T. ) ;
#17352 = DIRECTION ( 'NONE',  ( 1.000000000000000000, 0.000000000000000000, 0.000000000000000000 ) ) ;
#17353 = CYLINDRICAL_SURFACE ( 'NONE', #1027, 2.499999999999998668 ) ;
#17354 = FACE_OUTER_BOUND ( 'NONE', #5704, .T. ) ;
#17355 = CARTESIAN_POINT ( 'NONE',  ( -34.99999999999999289, 120.0000000000000284, -4.999999999999999112 ) ) ;
#17356 = LINE ( 'NONE', #5326, #9176 ) ;
#17357 = ORIENTED_EDGE ( 'NONE', *, *, #6682, .F. ) ;
#17358 = DIRECTION ( 'NONE',  ( 1.000000000000000000, 0.000000000000000000, 0.000000000000000000 ) ) ;
#17359 = CARTESIAN_POINT ( 'NONE',  ( -68.00000000000000000, 171.6227766016838245, 0.000000000000000000 ) ) ;
#17360 = ORIENTED_EDGE ( 'NONE', *, *, #2427, .T. ) ;
#17361 = DIRECTION ( 'NONE',  ( 1.000000000000000000, 0.000000000000000000, 0.000000000000000000 ) ) ;
#17362 = DIRECTION ( 'NONE',  ( 0.000000000000000000, 0.000000000000000000, 1.000000000000000000 ) ) ;
#17363 = EDGE_CURVE ( 'NONE', #9093, #9313, #11440, .T. ) ;
#17364 = VERTEX_POINT ( 'NONE', #10111 ) ;
#17365 = CARTESIAN_POINT ( 'NONE',  ( -8.720613081040568204, 20.00000000000000000, 24.99999999951824492 ) ) ;
#17366 = CARTESIAN_POINT ( 'NONE',  ( 26.13287303778632165, 139.7415755892579341, 8.533400866158022069 ) ) ;
#17367 = ORIENTED_EDGE ( 'NONE', *, *, #4576, .T. ) ;
#17368 = DIRECTION ( 'NONE',  ( 1.000000000000000000, 0.000000000000000000, 0.000000000000000000 ) ) ;
#17369 = VECTOR ( 'NONE', #7552, 1000.000000000000000 ) ;
#17370 = VERTEX_POINT ( 'NONE', #1150 ) ;
#17371 = AXIS2_PLACEMENT_3D ( 'NONE', #909, #15515, #4886 ) ;
#17372 = CARTESIAN_POINT ( 'NONE',  ( 15.00000000000903455, 143.2058235767352983, 16.77804593520375676 ) ) ;
#17373 = DIRECTION ( 'NONE',  ( -0.000000000000000000, -0.000000000000000000, 1.000000000000000000 ) ) ;
#17374 = CARTESIAN_POINT ( 'NONE',  ( 196.0000000000000000, 167.6227766016838530, 5.571800142134975431 ) ) ;
#17375 = CARTESIAN_POINT ( 'NONE',  ( -27.98221281341758626, 18.00000000000000000, -6.321711414556880904 ) ) ;
#17376 = ORIENTED_EDGE ( 'NONE', *, *, #3678, .F. ) ;
#17377 = CARTESIAN_POINT ( 'NONE',  ( 26.98389851090235680, 150.6144458722572779, 25.44936967851739595 ) ) ;
#17378 = VERTEX_POINT ( 'NONE', #16021 ) ;
#17379 = CARTESIAN_POINT ( 'NONE',  ( -73.64306072442659001, 192.6156044230848181, -25.46745035168474658 ) ) ;
#17380 = DIRECTION ( 'NONE',  ( 0.000000000000000000, 0.000000000000000000, 1.000000000000000000 ) ) ;
#17381 = AXIS2_PLACEMENT_3D ( 'NONE', #12239, #109, #10822 ) ;
#17382 = EDGE_CURVE ( 'NONE', #3326, #8820, #2577, .T. ) ;
#17383 = VERTEX_POINT ( 'NONE', #11853 ) ;
#17384 = EDGE_CURVE ( 'NONE', #17318, #4434, #17181, .T. ) ;
#17385 = CIRCLE ( 'NONE', #15680, 250.0000000000000000 ) ;
#17386 = VERTEX_POINT ( 'NONE', #15929 ) ;
#17387 = EDGE_CURVE ( 'NONE', #16273, #13530, #6439, .T. ) ;
#17388 = ORIENTED_EDGE ( 'NONE', *, *, #671, .F. ) ;
#17389 = CARTESIAN_POINT ( 'NONE',  ( 9.380362127004868711, 139.2112497869900949, 14.33999639901018242 ) ) ;
#17390 = ORIENTED_EDGE ( 'NONE', *, *, #13274, .F. ) ;
#17391 = CARTESIAN_POINT ( 'NONE',  ( 65.00000000000000000, 0.000000000000000000, 0.000000000000000000 ) ) ;
#17392 = DIRECTION ( 'NONE',  ( 0.000000000000000000, 0.000000000000000000, -1.000000000000000000 ) ) ;
#17393 = CARTESIAN_POINT ( 'NONE',  ( -168.3486229709906183, 182.2169359496550101, 0.000000000000000000 ) ) ;
#17394 = CIRCLE ( 'NONE', #13431, 10.00000000000000000 ) ;
#17395 = CARTESIAN_POINT ( 'NONE',  ( 39.99999999999998579, 20.00000000000000000, -30.00000000000001066 ) ) ;
#17396 = DIRECTION ( 'NONE',  ( 1.000000000000000000, 0.000000000000000000, 0.000000000000000000 ) ) ;
#17397 = CARTESIAN_POINT ( 'NONE',  ( -75.01941192507108269, 147.1381844727103214, 22.12819033745954300 ) ) ;
#17398 = PRESENTATION_LAYER_ASSIGNMENT (  '', '', ( #7494 ) ) ;
#17399 = VECTOR ( 'NONE', #16972, 1000.000000000000000 ) ;
#17400 = ORIENTED_EDGE ( 'NONE', *, *, #16063, .F. ) ;
#17401 = CARTESIAN_POINT ( 'NONE',  ( -77.50000000000001421, 196.6227766016838245, -16.00000000000000000 ) ) ;
#17402 = CARTESIAN_POINT ( 'NONE',  ( 0.000000000000000000, 0.8660254037844428154, -1.499999999999997780 ) ) ;
#17403 = CARTESIAN_POINT ( 'NONE',  ( 15.00000000000903455, 143.2885527162398489, -16.91661185963483760 ) ) ;
#17404 = PLANE ( 'NONE',  #10863 ) ;
#17405 = CARTESIAN_POINT ( 'NONE',  ( 17.21487247493544714, 29.96934980803111159, 14.74175109707249831 ) ) ;
#17406 = EDGE_LOOP ( 'NONE', ( #15293, #4991, #2251, #8175, #3594, #7095, #319, #13446 ) ) ;
#17407 = DIRECTION ( 'NONE',  ( 6.938893903907229364E-16, -0.000000000000000000, -1.000000000000000000 ) ) ;
#17408 = CIRCLE ( 'NONE', #1283, 7.500000000000007105 ) ;
#17409 = CARTESIAN_POINT ( 'NONE',  ( -48.00000000000000000, 171.6227766016838245, 0.000000000000000000 ) ) ;
#17410 = DIRECTION ( 'NONE',  ( 0.000000000000000000, 0.000000000000000000, -1.000000000000000000 ) ) ;
#17411 = AXIS2_PLACEMENT_3D ( 'NONE', #3434, #4669, #15374 ) ;
#17412 = VERTEX_POINT ( 'NONE', #4073 ) ;
#17413 = CARTESIAN_POINT ( 'NONE',  ( -68.00000000000000000, 171.6227766016838245, 20.00000000000000355 ) ) ;
#17414 = ORIENTED_EDGE ( 'NONE', *, *, #12575, .F. ) ;
#17415 = DIRECTION ( 'NONE',  ( -1.000000000000000000, 0.000000000000000000, 0.000000000000000000 ) ) ;
#17416 = LINE ( 'NONE', #12111, #14853 ) ;
#17417 = CARTESIAN_POINT ( 'NONE',  ( -76.51061601766232911, 141.7273756662291930, -18.20613184929476347 ) ) ;
#17418 = CARTESIAN_POINT ( 'NONE',  ( -8.719536044788661400, 19.99999999999999645, 24.99999999999999645 ) ) ;
#17419 = CLOSED_SHELL ( 'NONE', ( #16573, #4682, #5090, #13438, #9100, #14313, #245, #4364, #3753, #762, #13547, #4906, #15132, #16424, #8783, #5885, #2129, #14347, #11155, #15229, #12716, #6255, #10465, #16317, #336, #6268, #7844 ) ) ;
#17420 = AXIS2_PLACEMENT_3D ( 'NONE', #15781, #15874, #17026 ) ;
#17421 = EDGE_LOOP ( 'NONE', ( #4865, #2920 ) ) ;
#17422 = DIRECTION ( 'NONE',  ( -1.000000000000000000, -0.000000000000000000, -0.000000000000000000 ) ) ;
#17423 = FACE_OUTER_BOUND ( 'NONE', #16154, .T. ) ;
#17424 = CIRCLE ( 'NONE', #3283, 2.500000000000000000 ) ;
#17425 = LINE ( 'NONE', #4066, #12450 ) ;
#17426 = UNCERTAINTY_MEASURE_WITH_UNIT (LENGTH_MEASURE( 1.000000000000000082E-05 ), #3157, 'distance_accuracy_value', 'NONE');
#17427 = EDGE_CURVE ( 'NONE', #5867, #9898, #9286, .T. ) ;
#17428 = CARTESIAN_POINT ( 'NONE',  ( -151.0000000000000284, 171.6227766016838245, 0.000000000000000000 ) ) ;
#17429 = ORIENTED_EDGE ( 'NONE', *, *, #5189, .F. ) ;
#17430 = B_SPLINE_CURVE_WITH_KNOTS ( 'NONE', 3,
 ( #4448, #11252, #12766, #14186, #14007, #637, #13840, #15503, #1706, #12674, #16670, #13923 ),
 .UNSPECIFIED., .F., .F.,
 ( 4, 2, 2, 2, 2, 4 ),
 ( 0.000000000000000000, 0.0006954760458706877755, 0.001390952091741375551, 0.001738690114676747682, 0.002086428137612120030, 0.002781904183482844777 ),
 .UNSPECIFIED. ) ;
#17431 = DIRECTION ( 'NONE',  ( 0.000000000000000000, -1.000000000000000000, -6.123233995736762338E-17 ) ) ;
#17432 = ORIENTED_EDGE ( 'NONE', *, *, #994, .T. ) ;
#17433 = CARTESIAN_POINT ( 'NONE',  ( 17.00000000000000000, 143.0439382767972631, -16.49999999999984013 ) ) ;
#17434 = AXIS2_PLACEMENT_3D ( 'NONE', #5332, #9214, #13205 ) ;
#17435 = CARTESIAN_POINT ( 'NONE',  ( 26.13287303778632165, 139.7415755892579341, -8.533400866158022069 ) ) ;
#17436 = AXIS2_PLACEMENT_3D ( 'NONE', #5766, #9836, #4539 ) ;
#17437 = ORIENTED_EDGE ( 'NONE', *, *, #8405, .T. ) ;
#17438 = CARTESIAN_POINT ( 'NONE',  ( -74.72505082391211317, 201.9542783778900059, -13.00000000000000000 ) ) ;
#17439 = CIRCLE ( 'NONE', #6396, 20.00000000000000355 ) ;
#17440 = LINE ( 'NONE', #7775, #16417 ) ;
#17441 = VECTOR ( 'NONE', #3258, 1000.000000000000000 ) ;
#17442 = SHAPE_REPRESENTATION ( 'Brushless DC Motor Assembly', ( #3583 ), #12078 ) ;
#17443 = DIRECTION ( 'NONE',  ( 0.9961946980917463224, -0.04357787137382344855, -0.07547908730516518505 ) ) ;
#17444 = LINE ( 'NONE', #13192, #14604 ) ;
#17445 = CARTESIAN_POINT ( 'NONE',  ( 29.54149365486396661, 18.00000000000000355, -18.67620474358521676 ) ) ;
#17446 = CARTESIAN_POINT ( 'NONE',  ( 17.14315908062561533, 17.99999999999886313, -12.73566125713464636 ) ) ;
#17447 = DIRECTION ( 'NONE',  ( -1.000000000000000000, -0.000000000000000000, -0.000000000000000000 ) ) ;
#17448 = DIRECTION ( 'NONE',  ( -1.000000000000000000, 0.000000000000000000, 0.000000000000000000 ) ) ;
#17449 = CARTESIAN_POINT ( 'NONE',  ( -27.99999999999998224, 10.00000000000000000, -13.00000000000000000 ) ) ;
#17450 = ADVANCED_FACE ( 'NONE', ( #14603 ), #17261, .T. ) ;
#17451 = CARTESIAN_POINT ( 'NONE',  ( 27.99999999999998224, 9.999999999999998224, -12.99999999999999822 ) ) ;
#17452 = VERTEX_POINT ( 'NONE', #2381 ) ;
#17453 = CARTESIAN_POINT ( 'NONE',  ( 15.65639489742288681, 128.1581396164810940, -10.28488489824641761 ) ) ;
#17454 = CIRCLE ( 'NONE', #15466, 2.500000000000002220 ) ;
#17455 = VERTEX_POINT ( 'NONE', #17438 ) ;
#17456 = DIRECTION ( 'NONE',  ( -1.000000000000000000, 0.000000000000000000, 0.000000000000000000 ) ) ;
#17457 = CIRCLE ( 'NONE', #8695, 0.2000000000000000944 ) ;
#17458 = EDGE_CURVE ( 'NONE', #15092, #17193, #4417, .T. ) ;
#17459 = DIRECTION ( 'NONE',  ( 0.000000000000000000, 0.000000000000000000, -1.000000000000000000 ) ) ;
#17460 = ORIENTED_EDGE ( 'NONE', *, *, #13390, .T. ) ;
#17461 = EDGE_CURVE ( 'NONE', #15706, #11986, #17470, .T. ) ;
#17462 = CARTESIAN_POINT ( 'NONE',  ( -13.91527097789397160, 19.99999999999999645, 23.98152295253190758 ) ) ;
#17463 = ADVANCED_FACE ( 'NONE', ( #10525 ), #10437, .F. ) ;
#17464 = LINE ( 'NONE', #5335, #3115 ) ;
#17465 = ORIENTED_EDGE ( 'NONE', *, *, #15702, .T. ) ;
#17466 = DIRECTION ( 'NONE',  ( 1.000000000000000000, 0.000000000000000000, -0.000000000000000000 ) ) ;
#17467 = EDGE_LOOP ( 'NONE', ( #10925, #2451, #1439, #9826 ) ) ;
#17468 = VECTOR ( 'NONE', #4321, 1000.000000000000000 ) ;
#17469 = DIRECTION ( 'NONE',  ( 0.000000000000000000, 0.000000000000000000, -1.000000000000000000 ) ) ;
#17470 = CIRCLE ( 'NONE', #9824, 2.500000000000000000 ) ;
#17471 = CARTESIAN_POINT ( 'NONE',  ( -208.0711340499744324, 175.9387398585090523, 3.819775182827789717 ) ) ;
#17472 = CARTESIAN_POINT ( 'NONE',  ( 39.99999999999998579, -20.00000000000000000, 34.99999999999999289 ) ) ;
#17473 = EDGE_CURVE ( 'NONE', #8813, #15581, #215, .T. ) ;
#17474 = B_SPLINE_CURVE_WITH_KNOTS ( 'NONE', 3,
 ( #3804, #15853, #11856, #17263, #5408, #10527, #17174, #3905, #15933, #11946 ),
 .UNSPECIFIED., .F., .F.,
 ( 4, 2, 2, 2, 4 ),
 ( 2.030441771438897272E-17, 0.002588446031580682403, 0.005176892063161339652, 0.007765338094741996468, 0.01035378412632265502 ),
 .UNSPECIFIED. ) ;
#17475 = CARTESIAN_POINT ( 'NONE',  ( 49.99999999999998579, 155.6227766016839098, 10.00000337241049309 ) ) ;
#17476 = VERTEX_POINT ( 'NONE', #10797 ) ;
#17477 = CARTESIAN_POINT ( 'NONE',  ( 32.86958794498660552, 150.7324203247391381, 25.54751979981074683 ) ) ;
#17478 = VERTEX_POINT ( 'NONE', #15851 ) ;
#17479 = CARTESIAN_POINT ( 'NONE',  ( -25.00000000000002132, 100.0000000000000142, 4.999999999999999112 ) ) ;
#17480 = CARTESIAN_POINT ( 'NONE',  ( -87.04838423995398955, 199.2315236948359143, -18.09598853029520171 ) ) ;
#17481 = ORIENTED_EDGE ( 'NONE', *, *, #16955, .T. ) ;
#17482 = CIRCLE ( 'NONE', #10958, 30.00000000000000000 ) ;
#17483 = EDGE_LOOP ( 'NONE', ( #7997, #5063 ) ) ;
#17484 = ORIENTED_EDGE ( 'NONE', *, *, #7071, .F. ) ;
#17485 = AXIS2_PLACEMENT_3D ( 'NONE', #3726, #6555, #5140 ) ;
#17486 = DIRECTION ( 'NONE',  ( -1.000000000000000000, 0.000000000000000000, 0.000000000000000000 ) ) ;
#17487 = VERTEX_POINT ( 'NONE', #13452 ) ;
#17488 =( LENGTH_UNIT ( ) NAMED_UNIT ( * ) SI_UNIT ( .MILLI., .METRE. ) );
#17489 = CARTESIAN_POINT ( 'NONE',  ( 30.00000000000001066, 146.6227766016838245, 0.000000000000000000 ) ) ;
#17490 = CARTESIAN_POINT ( 'NONE',  ( -23.00000000000000000, 120.0000000000000284, 15.00000000000000000 ) ) ;
#17491 = CARTESIAN_POINT ( 'NONE',  ( 196.0000000000000000, 175.6227766016838245, 5.571800142134975431 ) ) ;
#17492 = EDGE_CURVE ( 'NONE', #4434, #17318, #8708, .T. ) ;
#17493 = CARTESIAN_POINT ( 'NONE',  ( -100.0000000000000000, 171.6227766016838245, 0.000000000000000000 ) ) ;
#17494 = ADVANCED_FACE ( 'NONE', ( #9452 ), #3902, .F. ) ;
#17495 = CARTESIAN_POINT ( 'NONE',  ( -75.76161824504397657, 149.2800176679284903, 24.28646496670947386 ) ) ;
#17496 = AXIS2_PLACEMENT_3D ( 'NONE', #11773, #14266, #2135 ) ;
#17497 = ADVANCED_FACE ( 'NONE', ( #5312 ), #12861, .F. ) ;
#17498 = CIRCLE ( 'NONE', #13825, 2.499999999999998668 ) ;
#17499 = ORIENTED_EDGE ( 'NONE', *, *, #14106, .T. ) ;
#17500 = LINE ( 'NONE', #17401, #4199 ) ;
#17501 = CARTESIAN_POINT ( 'NONE',  ( 15.60228996708978855, 124.9392590763941371, -1.387778780781445676E-14 ) ) ;
#17502 = CARTESIAN_POINT ( 'NONE',  ( 6.927042533203191965, 134.0880917650273716, 15.00000000000000533 ) ) ;
#17503 = CARTESIAN_POINT ( 'NONE',  ( 27.44407568426044008, 138.8271129316868837, -3.666666666666658081 ) ) ;
#17504 = DIRECTION ( 'NONE',  ( 0.000000000000000000, 0.000000000000000000, 1.000000000000000000 ) ) ;
#17505 = CARTESIAN_POINT ( 'NONE',  ( -50.00000000000000000, 171.6227766016838245, -19.49999999999998224 ) ) ;
#17506 = AXIS2_PLACEMENT_3D ( 'NONE', #7784, #17272, #5225 ) ;
#17507 = CYLINDRICAL_SURFACE ( 'NONE', #15555, 5.000000000000006217 ) ;
#17508 = CIRCLE ( 'NONE', #10423, 5.999999999999998224 ) ;
#17509 = EDGE_LOOP ( 'NONE', ( #1951, #12330, #5558 ) ) ;
#17510 = CARTESIAN_POINT ( 'NONE',  ( 33.99999999999998579, 9.999999999999998224, -16.00000000000000000 ) ) ;
#17511 = CIRCLE ( 'NONE', #547, 20.00000000000000355 ) ;
#17512 = ORIENTED_EDGE ( 'NONE', *, *, #12035, .T. ) ;
#17513 = APPLICATION_PROTOCOL_DEFINITION ( 'draft international standard', 'automotive_design', 1998, #5517 ) ;
#17514 = CARTESIAN_POINT ( 'NONE',  ( 15.93460003626534416, 136.8193095811534761, -3.708327557688629206 ) ) ;
#17515 = DIRECTION ( 'NONE',  ( 1.000000000000000000, -0.000000000000000000, -0.000000000000000000 ) ) ;
#17516 = CARTESIAN_POINT ( 'NONE',  ( -83.47886835550096407, 141.7198527106615984, -18.19376952932830349 ) ) ;
#17517 = EDGE_CURVE ( 'NONE', #539, #14780, #3613, .T. ) ;
#17518 = EDGE_CURVE ( 'NONE', #5075, #13335, #5875, .T. ) ;
#17519 = CARTESIAN_POINT ( 'NONE',  ( 49.99999999999998579, 191.6227766016837677, 8.071800142134975431 ) ) ;
#17520 = VERTEX_POINT ( 'NONE', #6460 ) ;
#17521 = CYLINDRICAL_SURFACE ( 'NONE', #14631, 2.499999999999998668 ) ;
#17522 = DIRECTION ( 'NONE',  ( -1.000000000000000000, 0.000000000000000000, 0.000000000000000000 ) ) ;
#17523 = NEXT_ASSEMBLY_USAGE_OCCURRENCE ( 'NAUO1', ' ', ' ', #7612, #3279, $ ) ;
#17524 = NEXT_ASSEMBLY_USAGE_OCCURRENCE ( 'NAUO2', ' ', ' ', #7612, #17347, $ ) ;
#17525 = NEXT_ASSEMBLY_USAGE_OCCURRENCE ( 'NAUO3', ' ', ' ', #7612, #5120, $ ) ;
#17526 = NEXT_ASSEMBLY_USAGE_OCCURRENCE ( 'NAUO4', ' ', ' ', #7612, #10297, $ ) ;
#17527 = NEXT_ASSEMBLY_USAGE_OCCURRENCE ( 'NAUO5', ' ', ' ', #7612, #4806, $ ) ;
#17528 = NEXT_ASSEMBLY_USAGE_OCCURRENCE ( 'NAUO6', ' ', ' ', #7612, #7065, $ ) ;
#17529 = NEXT_ASSEMBLY_USAGE_OCCURRENCE ( 'NAUO7', ' ', ' ', #7612, #1351, $ ) ;
#17530 = NEXT_ASSEMBLY_USAGE_OCCURRENCE ( 'NAUO8', ' ', ' ', #7612, #49, $ ) ;
#17531 = NEXT_ASSEMBLY_USAGE_OCCURRENCE ( 'NAUO9', ' ', ' ', #7612, #13343, $ ) ;
#17532 = NEXT_ASSEMBLY_USAGE_OCCURRENCE ( 'NAUO10', ' ', ' ', #7612, #4491, $ ) ;
#17533 = NEXT_ASSEMBLY_USAGE_OCCURRENCE ( 'NAUO11', ' ', ' ', #7612, #4491, $ ) ;
#17534 = NEXT_ASSEMBLY_USAGE_OCCURRENCE ( 'NAUO12', ' ', ' ', #7612, #4491, $ ) ;
#17535 = NEXT_ASSEMBLY_USAGE_OCCURRENCE ( 'NAUO13', ' ', ' ', #7612, #4491, $ ) ;
#17536 = NEXT_ASSEMBLY_USAGE_OCCURRENCE ( 'NAUO14', ' ', ' ', #7612, #4491, $ ) ;
#17537 = NEXT_ASSEMBLY_USAGE_OCCURRENCE ( 'NAUO15', ' ', ' ', #7612, #4491, $ ) ;
ENDSEC;
END-ISO-10303-21;
